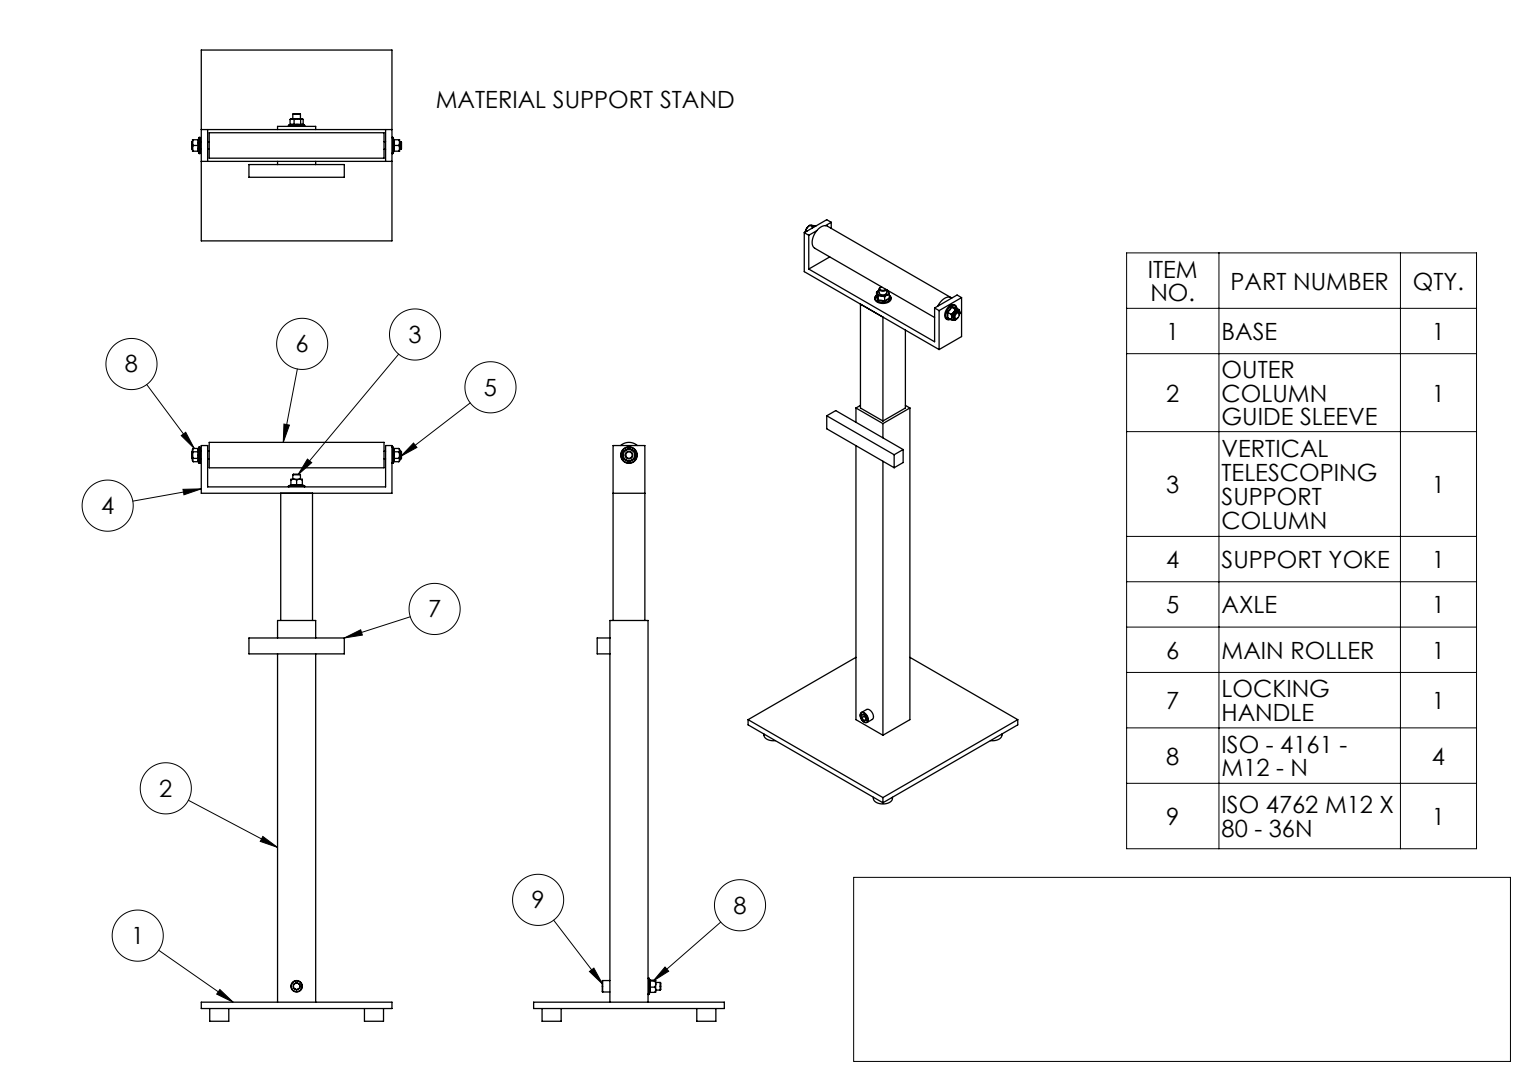
ISO-10303-21;
HEADER;
FILE_DESCRIPTION (('STEP AP214'),
    '1' );
FILE_NAME ('MAS-195',
    '2026-10-22T16:49:52',
    ( '' ),
    ( '' ),
    'SwSTEP 2.0',
    'SolidWorks 2026',
    '' );
FILE_SCHEMA (( 'AUTOMOTIVE_DESIGN' ));
ENDSEC;

DATA;
#1 = CARTESIAN_POINT ( 'NONE',  ( 6.000000000000000000, 5.839897972853065333, -6.938893903907228378E-15 ) ) ;
#2 = EDGE_LOOP ( 'NONE', ( #5035, #4306, #1396, #717 ) ) ;
#3 = ADVANCED_FACE ( 'NONE', ( #4862, #2431 ), #2781, .T. ) ;
#4 =( LENGTH_UNIT ( ) NAMED_UNIT ( * ) SI_UNIT ( .MILLI., .METRE. ) );
#5 = ORIENTED_EDGE ( 'NONE', *, *, #3129, .F. ) ;
#6 = AXIS2_PLACEMENT_3D ( 'NONE', #4882, #5186, #2714 ) ;
#7 = DIRECTION ( 'NONE',  ( 0.000000000000000000, 0.000000000000000000, -1.000000000000000000 ) ) ;
#8 = DIRECTION ( 'NONE',  ( -1.000000000000000000, -0.000000000000000000, -0.000000000000000000 ) ) ;
#9 = DIRECTION ( 'NONE',  ( 1.000000000000000000, -0.000000000000000000, 0.000000000000000000 ) ) ;
#10 = CONTEXT_DEPENDENT_SHAPE_REPRESENTATION ( #2601, #2272 ) ;
#11 = EDGE_CURVE ( 'NONE', #3738, #432, #4098, .T. ) ;
#12 = ORIENTED_EDGE ( 'NONE', *, *, #4828, .T. ) ;
#13 = DIRECTION ( 'NONE',  ( 7.401486830834378251E-16, -1.000000000000000000, 0.000000000000000000 ) ) ;
#14 = FACE_OUTER_BOUND ( 'NONE', #5143, .T. ) ;
#15 = DIRECTION ( 'NONE',  ( -1.000000000000000000, -0.000000000000000000, -0.000000000000000000 ) ) ;
#16 = EDGE_CURVE ( 'NONE', #5260, #261, #3181, .T. ) ;
#17 = CARTESIAN_POINT ( 'NONE',  ( 5.999999999999999112, -6.928203230275514102, -8.505011083697299412 ) ) ;
#18 = PRODUCT_DEFINITION_SHAPE ( 'NONE', 'NONE',  #4920 ) ;
#19 = APPLICATION_CONTEXT ( 'automotive_design' ) ;
#20 = EDGE_LOOP ( 'NONE', ( #1630, #2560 ) ) ;
#21 = CARTESIAN_POINT ( 'NONE',  ( 9.000000000000000000, -5.196152422706636465, -8.935996291721336249 ) ) ;
#22 = DIRECTION ( 'NONE',  ( -0.5000000000000046629, 1.060575238724903587E-16, -0.8660254037844359321 ) ) ;
#23 = ORIENTED_EDGE ( 'NONE', *, *, #198, .T. ) ;
#24 = EDGE_LOOP ( 'NONE', ( #1798, #2180 ) ) ;
#25 = CARTESIAN_POINT ( 'NONE',  ( 121.7157287525372311, 0.000000000000000000, -121.7157287525388369 ) ) ;
#26 = EDGE_LOOP ( 'NONE', ( #4357, #319, #2508, #4041 ) ) ;
#27 = ORIENTED_EDGE ( 'NONE', *, *, #3576, .T. ) ;
#28 = EDGE_LOOP ( 'NONE', ( #1037, #4864, #2855, #4479 ) ) ;
#29 = DIRECTION ( 'NONE',  ( 0.000000000000000000, -1.000000000000000000, 0.000000000000000000 ) ) ;
#30 = CARTESIAN_POINT ( 'NONE',  ( 150.0000000000000000, 810.0000000000000000, 25.00000000000000000 ) ) ;
#31 = CARTESIAN_POINT ( 'NONE',  ( 9.417977369734737536, -4.954833075775112228, -9.021743230619932774 ) ) ;
#32 = DIRECTION ( 'NONE',  ( 1.000000000000000000, -0.000000000000000000, 6.938893903907228378E-17 ) ) ;
#33 = EDGE_LOOP ( 'NONE', ( #4983, #5227 ) ) ;
#34 = DIRECTION ( 'NONE',  ( 1.000000000000000000, 0.000000000000000000, 0.000000000000000000 ) ) ;
#35 = SURFACE_SIDE_STYLE ('',( #3970 ) ) ;
#36 = LINE ( 'NONE', #4185, #4654 ) ;
#37 = CARTESIAN_POINT ( 'NONE',  ( -74.99999999999998579, 610.0000000000000000, 49.99999999999998579 ) ) ;
#38 = TOROIDAL_SURFACE ( 'NONE', #2294, 6.600000000000001421, 0.5999999999999999778 ) ;
#39 = EDGE_CURVE ( 'NONE', #183, #4714, #3882, .T. ) ;
#40 = AXIS2_PLACEMENT_3D ( 'NONE', #2568, #2148, #4717 ) ;
#41 = ORIENTED_EDGE ( 'NONE', *, *, #794, .F. ) ;
#42 = CARTESIAN_POINT ( 'NONE',  ( 149.9999999999999716, 10.00000000000000000, 149.9999999999999716 ) ) ;
#43 = CARTESIAN_POINT ( 'NONE',  ( 8.716942385998452281, -5.934590066575466061, -9.518277236634762772 ) ) ;
#44 = EDGE_LOOP ( 'NONE', ( #3924, #827, #3018, #2315, #3329 ) ) ;
#45 = EDGE_LOOP ( 'NONE', ( #4536, #2353, #4861, #2749 ) ) ;
#46 = VECTOR ( 'NONE', #2795, 1000.000000000000000 ) ;
#47 = MANIFOLD_SOLID_BREP ( 'M12 Machine Threads Stud2', #1956 ) ;
#48 = ORIENTED_EDGE ( 'NONE', *, *, #2007, .T. ) ;
#49 = CIRCLE ( 'NONE', #3968, 20.00000000000001421 ) ;
#50 = CARTESIAN_POINT ( 'NONE',  ( -150.0000000000000000, 870.0000000000000000, 0.000000000000000000 ) ) ;
#51 = VECTOR ( 'NONE', #3265, 1000.000000000000000 ) ;
#52 = EDGE_CURVE ( 'NONE', #4486, #4891, #4610, .T. ) ;
#53 = EDGE_LOOP ( 'NONE', ( #12, #4860, #912, #4381 ) ) ;
#54 = AXIS2_PLACEMENT_3D ( 'NONE', #1971, #1612, #2923 ) ;
#55 = DIRECTION ( 'NONE',  ( 0.000000000000000000, -0.000000000000000000, 1.000000000000000000 ) ) ;
#56 = CARTESIAN_POINT ( 'NONE',  ( -5.303004762135290484, 7.330613618480585458, -8.460795847313656637 ) ) ;
#57 = LINE ( 'NONE', #1683, #3118 ) ;
#58 = ADVANCED_FACE ( 'NONE', ( #1562 ), #1695, .F. ) ;
#59 = CIRCLE ( 'NONE', #3730, 6.499999999999983125 ) ;
#60 = CIRCLE ( 'NONE', #4076, 6.600000000000001421 ) ;
#61 = CARTESIAN_POINT ( 'NONE',  ( -24.99999999999999645, 810.0000000000000000, -25.00000000000000000 ) ) ;
#62 = DIRECTION ( 'NONE',  ( -0.000000000000000000, -0.000000000000000000, 1.000000000000000000 ) ) ;
#63 = CARTESIAN_POINT ( 'NONE',  ( 137.5000000000000000, 870.0000000000000000, 6.000000000000006217 ) ) ;
#64 = DIRECTION ( 'NONE',  ( -0.000000000000000000, -0.000000000000000000, 1.000000000000000000 ) ) ;
#65 = LINE ( 'NONE', #137, #1780 ) ;
#66 = EDGE_LOOP ( 'NONE', ( #727, #5386, #2171, #4175 ) ) ;
#67=STYLED_ITEM('',(#5412),#3780);
#68 = SURFACE_STYLE_FILL_AREA ( #524 ) ;
#69 = EDGE_CURVE ( 'NONE', #3352, #3493, #3834, .T. ) ;
#70 = VECTOR ( 'NONE', #4320, 1000.000000000000000 ) ;
#71 = EDGE_LOOP ( 'NONE', ( #1973, #4142, #2111, #5305 ) ) ;
#72 = CARTESIAN_POINT ( 'NONE',  ( -150.0000000000000000, 820.0000000000001137, 25.00000000000000000 ) ) ;
#73 = DIRECTION ( 'NONE',  ( 0.000000000000000000, 0.000000000000000000, -1.000000000000000000 ) ) ;
#74 = DIRECTION ( 'NONE',  ( 1.000000000000000000, 0.000000000000000000, 0.000000000000000000 ) ) ;
#75 = ORIENTED_EDGE ( 'NONE', *, *, #1128, .F. ) ;
#76 = CIRCLE ( 'NONE', #4758, 20.00000000000001421 ) ;
#77 = AXIS2_PLACEMENT_3D ( 'NONE', #4332, #3953, #3470 ) ;
#78 = DIRECTION ( 'NONE',  ( -6.938893903907228378E-17, 0.000000000000000000, 1.000000000000000000 ) ) ;
#79 = EDGE_CURVE ( 'NONE', #3280, #3385, #2552, .T. ) ;
#80 = EDGE_CURVE ( 'NONE', #4039, #3851, #2630, .T. ) ;
#81 = VERTEX_POINT ( 'NONE', #3427 ) ;
#82 = ORIENTED_EDGE ( 'NONE', *, *, #2566, .T. ) ;
#83 = LINE ( 'NONE', #4223, #2397 ) ;
#84 = DIRECTION ( 'NONE',  ( 2.081668171172168513E-16, 0.000000000000000000, -1.000000000000000000 ) ) ;
#85 = FACE_OUTER_BOUND ( 'NONE', #3426, .T. ) ;
#86 = CARTESIAN_POINT ( 'NONE',  ( -0.3334815747005946962, -10.58484052233643702, -9.543752552345290852 ) ) ;
#87 = CARTESIAN_POINT ( 'NONE',  ( -17.99999999999999645, -3.469446951953614189E-15, 0.000000000000000000 ) ) ;
#88 = LINE ( 'NONE', #3399, #4556 ) ;
#89 = DIRECTION ( 'NONE',  ( 1.000000000000000000, 0.000000000000000000, 0.000000000000000000 ) ) ;
#90 = CARTESIAN_POINT ( 'NONE',  ( 0.000000000000000000, 0.000000000000000000, -12.00000000000000000 ) ) ;
#91 = CARTESIAN_POINT ( 'NONE',  ( 5.099999999999999645, 0.000000000000000000, -0.6301867843887398735 ) ) ;
#92 = ORIENTED_EDGE ( 'NONE', *, *, #352, .F. ) ;
#93 = DIRECTION ( 'NONE',  ( -1.000000000000000000, -0.000000000000000000, -0.000000000000000000 ) ) ;
#94 = CARTESIAN_POINT ( 'NONE',  ( 7.780966735391740663, 5.899961606179080498, -9.200452032548549042 ) ) ;
#95 = UNCERTAINTY_MEASURE_WITH_UNIT (LENGTH_MEASURE( 1.000000000000000082E-05 ), #3819, 'distance_accuracy_value', 'NONE');
#96 = CARTESIAN_POINT ( 'NONE',  ( 3.148120153201419136, -9.125992800952634099, -9.189707035345831443 ) ) ;
#97 = CARTESIAN_POINT ( 'NONE',  ( 0.000000000000000000, 810.0000000000000000, 0.000000000000000000 ) ) ;
#98 = EDGE_CURVE ( 'NONE', #1888, #3300, #2243, .T. ) ;
#99 = ORIENTED_EDGE ( 'NONE', *, *, #4103, .T. ) ;
#100 = CARTESIAN_POINT ( 'NONE',  ( 0.000000000000000000, 0.000000000000000000, 0.000000000000000000 ) ) ;
#101 = DIRECTION ( 'NONE',  ( 0.000000000000000000, 0.000000000000000000, 1.000000000000000000 ) ) ;
#102 = CARTESIAN_POINT ( 'NONE',  ( 24.99999999999999645, 60.00000000000000711, -25.00000000000000000 ) ) ;
#103 = DIRECTION ( 'NONE',  ( 1.000000000000000000, 0.000000000000000000, 0.000000000000000000 ) ) ;
#104 = MANIFOLD_SOLID_BREP ( 'M12 Clearance Hole1', #2049 ) ;
#105 = CARTESIAN_POINT ( 'NONE',  ( 9.506737344437272696, -5.488717364925930653, -9.686084310752812954 ) ) ;
#106 = DIRECTION ( 'NONE',  ( 1.000000000000000000, 0.000000000000000000, 0.000000000000000000 ) ) ;
#107 = CARTESIAN_POINT ( 'NONE',  ( -3.715831927071960639, 8.246968282054856658, 1.905824131322174974E-15 ) ) ;
#108 = LINE ( 'NONE', #1461, #5040 ) ;
#109 = APPLICATION_CONTEXT ( 'automotive_design' ) ;
#110 = EDGE_CURVE ( 'NONE', #2103, #3079, #2190, .T. ) ;
#111 = CARTESIAN_POINT ( 'NONE',  ( -150.0000000000000284, 10.00000000000000000, 149.9999999999999147 ) ) ;
#112 = PLANE ( 'NONE',  #5289 ) ;
#113 = CARTESIAN_POINT ( 'NONE',  ( 9.333481574700595473, 5.003616745783458164, -9.543752552345289075 ) ) ;
#114 = DIRECTION ( 'NONE',  ( 1.000000000000000000, 0.000000000000000000, 0.000000000000000000 ) ) ;
#115 = EDGE_CURVE ( 'NONE', #4871, #4344, #3809, .T. ) ;
#116 = VECTOR ( 'NONE', #4178, 1000.000000000000000 ) ;
#117 = CARTESIAN_POINT ( 'NONE',  ( -121.7157287525381122, -20.00000000000000000, 106.7157287525380127 ) ) ;
#118 = CIRCLE ( 'NONE', #3006, 6.499999999999988454 ) ;
#119 = ADVANCED_BREP_SHAPE_REPRESENTATION ( '', ( #1812, #4154 ), #5370 ) ;
#120 = EDGE_LOOP ( 'NONE', ( #3988, #3057, #2483, #2092 ) ) ;
#121 = SHAPE_REPRESENTATION ( 'Locking handle', ( #4154 ), #2227 ) ;
#122 = AXIS2_PLACEMENT_3D ( 'NONE', #2468, #3586, #4820 ) ;
#123 = ORIENTED_EDGE ( 'NONE', *, *, #1408, .F. ) ;
#124 = DIRECTION ( 'NONE',  ( 1.224646799147353207E-16, 1.000000000000000000, 0.000000000000000000 ) ) ;
#125 = CARTESIAN_POINT ( 'NONE',  ( 92.00000000000000000, 0.000000000000000000, 5.035999999999999588 ) ) ;
#126 = EDGE_CURVE ( 'NONE', #4344, #870, #2364, .T. ) ;
#127 = DIRECTION ( 'NONE',  ( -0.000000000000000000, -0.000000000000000000, 1.000000000000000000 ) ) ;
#128 = VECTOR ( 'NONE', #1979, 1000.000000000000000 ) ;
#129 = CIRCLE ( 'NONE', #3889, 6.000000000000000000 ) ;
#130 = AXIS2_PLACEMENT_3D ( 'NONE', #2726, #4867, #1140 ) ;
#131 = CARTESIAN_POINT ( 'NONE',  ( -8.999999999999998224, 4.786605659887710473, -1.023509873932516578 ) ) ;
#132 = CARTESIAN_POINT ( 'NONE',  ( 165.0000000000000000, 870.0000000000000000, -5.036000000000040444 ) ) ;
#133 = DIRECTION ( 'NONE',  ( 1.000000000000000000, 0.000000000000000000, 0.000000000000000000 ) ) ;
#134 = CARTESIAN_POINT ( 'NONE',  ( 30.00000000000000355, 610.0000000000000000, 30.00000000000001066 ) ) ;
#135 = ORIENTED_EDGE ( 'NONE', *, *, #3214, .F. ) ;
#136 = EDGE_CURVE ( 'NONE', #4283, #3488, #3860, .T. ) ;
#137 = CARTESIAN_POINT ( 'NONE',  ( -24.99999999999999645, 610.0000000000000000, -25.00000000000000000 ) ) ;
#138 = DIRECTION ( 'NONE',  ( 0.000000000000000000, 0.000000000000000000, 1.000000000000000000 ) ) ;
#139 = EDGE_CURVE ( 'NONE', #2539, #1113, #5108, .T. ) ;
#140 = AXIS2_PLACEMENT_3D ( 'NONE', #4031, #279, #2385 ) ;
#141 = COLOUR_RGB ( '',0.8941176470588234615, 0.8941176470588234615, 0.8941176470588234615 ) ;
#142 = CARTESIAN_POINT ( 'NONE',  ( 6.000000000000000000, 5.839897972853065333, -6.938893903907228378E-15 ) ) ;
#143 = DIRECTION ( 'NONE',  ( 0.000000000000000000, 0.000000000000000000, -1.000000000000000000 ) ) ;
#144 = CARTESIAN_POINT ( 'NONE',  ( 0.000000000000000000, 570.0000000000000000, 25.00000000000000000 ) ) ;
#145 = VECTOR ( 'NONE', #5158, 1000.000000000000000 ) ;
#146 = CARTESIAN_POINT ( 'NONE',  ( -74.99999999999998579, 582.4999999999997726, 49.99999999999998579 ) ) ;
#147 = CARTESIAN_POINT ( 'NONE',  ( -121.7157287525381122, 0.000000000000000000, 106.7157287525380127 ) ) ;
#148 = VECTOR ( 'NONE', #4543, 1000.000000000000000 ) ;
#149 = CARTESIAN_POINT ( 'NONE',  ( 0.000000000000000000, -2.919948986426539772, -5.057499999999996554 ) ) ;
#150 = VECTOR ( 'NONE', #4769, 1000.000000000000000 ) ;
#151 = ORIENTED_EDGE ( 'NONE', *, *, #3972, .F. ) ;
#152 = SURFACE_STYLE_USAGE ( .BOTH. , #2636 ) ;
#153 = ORIENTED_EDGE ( 'NONE', *, *, #5054, .F. ) ;
#154 = VECTOR ( 'NONE', #5264, 1000.000000000000000 ) ;
#155 = ORIENTED_EDGE ( 'NONE', *, *, #2076, .F. ) ;
#156 = EDGE_CURVE ( 'NONE', #870, #4344, #3054, .T. ) ;
#157 = SURFACE_SIDE_STYLE ('',( #4715 ) ) ;
#158 = LINE ( 'NONE', #4749, #4217 ) ;
#159 = CARTESIAN_POINT ( 'NONE',  ( 6.000000000000000000, -5.258101095580057102E-15, -5.057500000000000107 ) ) ;
#160 = ORIENTED_EDGE ( 'NONE', *, *, #3298, .F. ) ;
#161 = ORIENTED_EDGE ( 'NONE', *, *, #5198, .T. ) ;
#162 = CARTESIAN_POINT ( 'NONE',  ( -150.0000000000000000, 870.0000000000000000, -6.000000000000006217 ) ) ;
#163 = FACE_OUTER_BOUND ( 'NONE', #2172, .T. ) ;
#164 = DIRECTION ( 'NONE',  ( -0.000000000000000000, -0.000000000000000000, 1.000000000000000000 ) ) ;
#165 = VERTEX_POINT ( 'NONE', #2690 ) ;
#166 = CARTESIAN_POINT ( 'NONE',  ( 9.000000000000000000, -5.196152422706636465, -8.935996291721336249 ) ) ;
#167 = EDGE_CURVE ( 'NONE', #2868, #5294, #475, .T. ) ;
#168 = CARTESIAN_POINT ( 'NONE',  ( 8.999999999999998224, -3.085342593989931714, -0.4353033105082919074 ) ) ;
#169 = ORIENTED_EDGE ( 'NONE', *, *, #1169, .T. ) ;
#170 = DIRECTION ( 'NONE',  ( 0.000000000000000000, -0.5000000000000012212, -0.8660254037844380415 ) ) ;
#171 = CARTESIAN_POINT ( 'NONE',  ( 5.010000000000002451, 0.000000000000000000, -0.6932054628276118624 ) ) ;
#172 = MECHANICAL_DESIGN_GEOMETRIC_PRESENTATION_REPRESENTATION (  '', ( #4869 ), #4866 ) ;
#173 = CARTESIAN_POINT ( 'NONE',  ( 12.38940648156203927, 1.517264699098042146E-15, -10.20000000000000107 ) ) ;
#174 = DIRECTION ( 'NONE',  ( -1.000000000000000000, 0.000000000000000000, 0.000000000000000000 ) ) ;
#175 = CARTESIAN_POINT ( 'NONE',  ( 8.999999999999998224, 5.582890641074283344, -9.544071791823135698 ) ) ;
#176 = CARTESIAN_POINT ( 'NONE',  ( 7.500000000000000000, 6.062177826491069510, -8.667800885990208926 ) ) ;
#177 = ORIENTED_EDGE ( 'NONE', *, *, #2712, .T. ) ;
#178 =( NAMED_UNIT ( * ) SI_UNIT ( $, .STERADIAN. ) SOLID_ANGLE_UNIT ( ) );
#179 = EDGE_CURVE ( 'NONE', #353, #1195, #2907, .T. ) ;
#180 = CARTESIAN_POINT ( 'NONE',  ( 0.000000000000000000, 0.000000000000000000, 0.000000000000000000 ) ) ;
#181 = CARTESIAN_POINT ( 'NONE',  ( 0.000000000000000000, 450.0000000000000000, 25.00000000000000000 ) ) ;
#182 = PRODUCT_DEFINITION ( 'UNKNOWN', '', #3186, #2002 ) ;
#183 = VERTEX_POINT ( 'NONE', #3483 ) ;
#184 = CARTESIAN_POINT ( 'NONE',  ( -121.7157287525381122, 0.000000000000000000, 121.7157287525380127 ) ) ;
#185 = CARTESIAN_POINT ( 'NONE',  ( -9.000000000000000000, 5.196152422706629359, -8.935996291721334472 ) ) ;
#186 = LINE ( 'NONE', #5103, #588 ) ;
#187 = CARTESIAN_POINT ( 'NONE',  ( 162.0000000000000000, 870.0000000000000000, 0.000000000000000000 ) ) ;
#188 = EDGE_LOOP ( 'NONE', ( #4329, #3309, #4220, #3176 ) ) ;
#189 = DIRECTION ( 'NONE',  ( -1.000000000000000000, -0.000000000000000000, -0.000000000000000000 ) ) ;
#190 = SURFACE_STYLE_FILL_AREA ( #1881 ) ;
#191 = DIRECTION ( 'NONE',  ( -0.000000000000000000, -1.000000000000000000, 0.000000000000000000 ) ) ;
#192 = DIRECTION ( 'NONE',  ( -0.000000000000000000, 1.000000000000000000, -0.000000000000000000 ) ) ;
#193 = FACE_OUTER_BOUND ( 'NONE', #4538, .T. ) ;
#194 = EDGE_CURVE ( 'NONE', #2394, #3572, #803, .T. ) ;
#195 = CARTESIAN_POINT ( 'NONE',  ( 165.0000000000000000, 870.0000000000000000, 5.036000000000040444 ) ) ;
#196 = DIRECTION ( 'NONE',  ( -0.000000000000000000, 1.000000000000000000, -0.000000000000000000 ) ) ;
#197 = ORIENTED_EDGE ( 'NONE', *, *, #3520, .F. ) ;
#198 = EDGE_CURVE ( 'NONE', #3942, #4623, #5254, .T. ) ;
#199 = CONICAL_SURFACE ( 'NONE', #1255, 5.036000000000040444, 0.7853981633974339571 ) ;
#200 = ORIENTED_EDGE ( 'NONE', *, *, #4627, .T. ) ;
#201 = CARTESIAN_POINT ( 'NONE',  ( 121.7157287525384533, -20.00000000000000000, 121.7157287525376859 ) ) ;
#202 = ORIENTED_EDGE ( 'NONE', *, *, #4322, .T. ) ;
#203 = DIRECTION ( 'NONE',  ( 0.000000000000000000, 0.000000000000000000, -1.000000000000000000 ) ) ;
#204 = CARTESIAN_POINT ( 'NONE',  ( 0.000000000000000000, 450.0000000000000000, -25.00000000000000000 ) ) ;
#205 = COLOUR_RGB ( '',1.000000000000000000, 0.9490196078431372140, 0.9098039215686274384 ) ;
#206 = EDGE_CURVE ( 'NONE', #3842, #5043, #2268, .T. ) ;
#207 = VERTEX_POINT ( 'NONE', #1151 ) ;
#208 = AXIS2_PLACEMENT_3D ( 'NONE', #1676, #429, #2877 ) ;
#209 = CARTESIAN_POINT ( 'NONE',  ( -9.506737344437272696, 5.488717364925923548, -9.686084310752812954 ) ) ;
#210 = CARTESIAN_POINT ( 'NONE',  ( 5.035999999999999588, 840.0000000000001137, 0.000000000000000000 ) ) ;
#211 = EDGE_CURVE ( 'NONE', #2103, #3135, #3145, .T. ) ;
#212 = ADVANCED_FACE ( 'NONE', ( #4821, #5247 ), #1493, .F. ) ;
#213 = DIRECTION ( 'NONE',  ( -1.000000000000000000, 0.000000000000000000, -2.081668171172168513E-16 ) ) ;
#214 = CARTESIAN_POINT ( 'NONE',  ( 9.000000000000007105, -5.196152422706631135, -9.106324069981642566 ) ) ;
#215 = FILL_AREA_STYLE ('',( #650 ) ) ;
#216 = AXIS2_PLACEMENT_3D ( 'NONE', #2652, #2351, #4049 ) ;
#217 = CIRCLE ( 'NONE', #2845, 6.499999999999988454 ) ;
#218 = PRESENTATION_LAYER_ASSIGNMENT (  '', '', ( #3627 ) ) ;
#219 = CARTESIAN_POINT ( 'NONE',  ( 8.919948986426568638, 0.000000000000000000, 0.000000000000000000 ) ) ;
#220 = ORIENTED_EDGE ( 'NONE', *, *, #4751, .F. ) ;
#221 = CARTESIAN_POINT ( 'NONE',  ( -3.936978610624180419, -8.666338374798538524, -9.138972935415381471 ) ) ;
#222 = CARTESIAN_POINT ( 'NONE',  ( 4.105894441359817293, 8.021765584429983775, 1.987139294258588595E-15 ) ) ;
#223 = ADVANCED_FACE ( 'NONE', ( #720 ), #3527, .F. ) ;
#224 = DIRECTION ( 'NONE',  ( 0.000000000000000000, 0.000000000000000000, -1.000000000000000000 ) ) ;
#225 = DIRECTION ( 'NONE',  ( -0.000000000000000000, 1.000000000000000000, -0.000000000000000000 ) ) ;
#226 = CIRCLE ( 'NONE', #1785, 6.499999999999988454 ) ;
#227 =( GEOMETRIC_REPRESENTATION_CONTEXT ( 3 ) GLOBAL_UNCERTAINTY_ASSIGNED_CONTEXT ( ( #1775 ) ) GLOBAL_UNIT_ASSIGNED_CONTEXT ( ( #3570, #5196, #2363 ) ) REPRESENTATION_CONTEXT ( 'NONE', 'WORKASPACE' ) );
#228 = AXIS2_PLACEMENT_3D ( 'NONE', #622, #648, #2683 ) ;
#229 = MECHANICAL_DESIGN_GEOMETRIC_PRESENTATION_REPRESENTATION (  '', ( #3546 ), #1970 ) ;
#230 = CARTESIAN_POINT ( 'NONE',  ( 9.000000000000000000, -1.974011471328773748, -8.465140122390733879 ) ) ;
#231 = PLANE ( 'NONE',  #3894 ) ;
#232 = VECTOR ( 'NONE', #2038, 1000.000000000000000 ) ;
#233 = EDGE_CURVE ( 'NONE', #932, #4959, #723, .T. ) ;
#234 = VECTOR ( 'NONE', #2330, 1000.000000000000000 ) ;
#235 = ORIENTED_EDGE ( 'NONE', *, *, #3529, .T. ) ;
#236 = CYLINDRICAL_SURFACE ( 'NONE', #2573, 6.499999999999983125 ) ;
#237 = ADVANCED_FACE ( 'NONE', ( #3202, #2295 ), #602, .T. ) ;
#238 = ORIENTED_EDGE ( 'NONE', *, *, #1651, .F. ) ;
#239 = DIRECTION ( 'NONE',  ( -1.000000000000000000, -0.000000000000000000, -0.000000000000000000 ) ) ;
#240 = FACE_OUTER_BOUND ( 'NONE', #4695, .T. ) ;
#241 = AXIS2_PLACEMENT_3D ( 'NONE', #2577, #882, #3403 ) ;
#242 = ORIENTED_EDGE ( 'NONE', *, *, #1915, .F. ) ;
#243 = DIRECTION ( 'NONE',  ( -1.000000000000000000, -0.000000000000000000, -0.000000000000000000 ) ) ;
#244 = CARTESIAN_POINT ( 'NONE',  ( -6.177322775498885754, -6.825825878106156708, -8.969375302469426714 ) ) ;
#245 = CIRCLE ( 'NONE', #77, 6.000000000000006217 ) ;
#246 = CARTESIAN_POINT ( 'NONE',  ( 6.000000000000000000, -5.839897972853064445, 4.770489558936219510E-15 ) ) ;
#247 = CARTESIAN_POINT ( 'NONE',  ( 139.9999999999999716, 885.0000000000000000, -25.00000000000000000 ) ) ;
#248 = DIRECTION ( 'NONE',  ( 0.000000000000000000, 0.000000000000000000, 1.000000000000000000 ) ) ;
#249 = ORIENTED_EDGE ( 'NONE', *, *, #342, .F. ) ;
#250 = CARTESIAN_POINT ( 'NONE',  ( 9.000000000000000000, -4.368650009232623255, -0.8589767385557531831 ) ) ;
#251 = CARTESIAN_POINT ( 'NONE',  ( 0.000000000000000000, 0.000000000000000000, 0.000000000000000000 ) ) ;
#252 = CARTESIAN_POINT ( 'NONE',  ( -0.7813822207450746848, 10.51618336147351584, -9.518202542148552325 ) ) ;
#253 = DIRECTION ( 'NONE',  ( 1.000000000000000000, 0.000000000000000000, 0.000000000000000000 ) ) ;
#254 = CARTESIAN_POINT ( 'NONE',  ( -150.0000000000000284, 0.000000000000000000, 149.9999999999999147 ) ) ;
#255 = PRODUCT_DEFINITION ( 'UNKNOWN', '', #483, #2329 ) ;
#256 = CARTESIAN_POINT ( 'NONE',  ( 8.999999999999998224, 3.726892940488169881, -9.220324059310399889 ) ) ;
#257 = CARTESIAN_POINT ( 'NONE',  ( 30.00000000000000355, 610.0000000000000000, 30.00000000000001066 ) ) ;
#258 = MANIFOLD_SOLID_BREP ( 'M12 Machine Threads Stud1', #3451 ) ;
#259 = ORIENTED_EDGE ( 'NONE', *, *, #2872, .T. ) ;
#260 = FACE_OUTER_BOUND ( 'NONE', #4753, .T. ) ;
#261 = VERTEX_POINT ( 'NONE', #1126 ) ;
#262 = DIRECTION ( 'NONE',  ( 1.000000000000000000, 0.000000000000000000, 0.000000000000000000 ) ) ;
#263 = DIRECTION ( 'NONE',  ( 0.000000000000000000, 0.000000000000000000, 1.000000000000000000 ) ) ;
#264 = ADVANCED_FACE ( 'NONE', ( #307 ), #2257, .T. ) ;
#265 = EDGE_LOOP ( 'NONE', ( #2371, #2953, #3859, #3002, #619 ) ) ;
#266 = EDGE_CURVE ( 'NONE', #4086, #2529, #4435, .T. ) ;
#267 = ORIENTED_EDGE ( 'NONE', *, *, #3062, .T. ) ;
#268 = CARTESIAN_POINT ( 'NONE',  ( -12.07201791628681420, 1.497830254570528423E-15, -12.00000000000000178 ) ) ;
#269 = DIRECTION ( 'NONE',  ( 0.000000000000000000, 0.000000000000000000, -1.000000000000000000 ) ) ;
#270 = CARTESIAN_POINT ( 'NONE',  ( 9.473745496805531019, 0.9193675319299579041, -9.138786188337409300 ) ) ;
#271 = CARTESIAN_POINT ( 'NONE',  ( 6.499999999999988454, 450.0000000000000000, -25.00000000000000000 ) ) ;
#272 = APPLICATION_PROTOCOL_DEFINITION ( 'draft international standard', 'automotive_design', 1998, #5061 ) ;
#273 = VERTEX_POINT ( 'NONE', #4446 ) ;
#274 = B_SPLINE_CURVE_WITH_KNOTS ( 'NONE', 3,
 ( #1691, #107, #2527, #1724, #4580, #2576 ),
 .UNSPECIFIED., .F., .F.,
 ( 4, 2, 4 ),
 ( 0.005333245961717295557, 0.007986067645924077585, 0.01063888933013085875 ),
 .UNSPECIFIED. ) ;
#275 = DIRECTION ( 'NONE',  ( 1.000000000000000000, 0.000000000000000000, 0.000000000000000000 ) ) ;
#276 = ORIENTED_EDGE ( 'NONE', *, *, #1791, .T. ) ;
#277 = CARTESIAN_POINT ( 'NONE',  ( -3.145304002162441659, -9.127642243957643231, -9.190020220263408035 ) ) ;
#278 = CYLINDRICAL_SURFACE ( 'NONE', #4326, 9.000000000000000000 ) ;
#279 = DIRECTION ( 'NONE',  ( -0.000000000000000000, -0.000000000000000000, 1.000000000000000000 ) ) ;
#280 = CARTESIAN_POINT ( 'NONE',  ( 139.9999999999999716, 885.0000000000000000, 25.00000000000000000 ) ) ;
#281 = ADVANCED_FACE ( 'NONE', ( #2796 ), #733, .T. ) ;
#282 = LINE ( 'NONE', #1853, #2054 ) ;
#283 = DIRECTION ( 'NONE',  ( -0.000000000000000000, -0.000000000000000000, 1.000000000000000000 ) ) ;
#284 = EDGE_CURVE ( 'NONE', #3602, #4122, #385, .T. ) ;
#285 = VERTEX_POINT ( 'NONE', #3734 ) ;
#286 = EDGE_LOOP ( 'NONE', ( #1725, #726, #2392, #4939 ) ) ;
#287 = APPLICATION_CONTEXT ( 'automotive_design' ) ;
#288 = PRESENTATION_STYLE_ASSIGNMENT (( #4836 ) ) ;
#289 = DIRECTION ( 'NONE',  ( 0.000000000000000000, 0.000000000000000000, 1.000000000000000000 ) ) ;
#290 = AXIS2_PLACEMENT_3D ( 'NONE', #2542, #2961, #4599 ) ;
#291 = EDGE_LOOP ( 'NONE', ( #3664, #547 ) ) ;
#292 = DIRECTION ( 'NONE',  ( -0.5000000000000004441, 0.8660254037844384856, 0.000000000000000000 ) ) ;
#293 = FACE_OUTER_BOUND ( 'NONE', #4919, .T. ) ;
#294 = EDGE_LOOP ( 'NONE', ( #2275, #2236, #92, #4689 ) ) ;
#295 = AXIS2_PLACEMENT_3D ( 'NONE', #2964, #518, #4278 ) ;
#296 = ORIENTED_EDGE ( 'NONE', *, *, #4163, .F. ) ;
#297 = DIRECTION ( 'NONE',  ( 0.000000000000000000, -1.000000000000000000, 0.000000000000000000 ) ) ;
#298 = CARTESIAN_POINT ( 'NONE',  ( 164.0360000000000014, 870.0000000000000000, -6.000000000000006217 ) ) ;
#299 = DIRECTION ( 'NONE',  ( -0.000000000000000000, -0.000000000000000000, 1.000000000000000000 ) ) ;
#300 = VECTOR ( 'NONE', #2784, 1000.000000000000000 ) ;
#301 = UNCERTAINTY_MEASURE_WITH_UNIT (LENGTH_MEASURE( 1.000000000000000082E-05 ), #2011, 'distance_accuracy_value', 'NONE');
#302 = SHAPE_REPRESENTATION ( 'axle', ( #4154 ), #2055 ) ;
#303 = ORIENTED_EDGE ( 'NONE', *, *, #2481, .F. ) ;
#304 = AXIS2_PLACEMENT_3D ( 'NONE', #2018, #4467, #1392 ) ;
#305 = ADVANCED_FACE ( 'NONE', ( #1215, #3776 ), #1663, .T. ) ;
#306 = DIRECTION ( 'NONE',  ( 1.000000000000000000, 0.000000000000000000, -0.000000000000000000 ) ) ;
#307 = FACE_OUTER_BOUND ( 'NONE', #4376, .T. ) ;
#308 = SURFACE_STYLE_USAGE ( .BOTH. , #4112 ) ;
#309 = CARTESIAN_POINT ( 'NONE',  ( -137.5000000000000000, 870.0000000000000000, 0.000000000000000000 ) ) ;
#310 = EDGE_CURVE ( 'NONE', #3078, #932, #2677, .T. ) ;
#311 = DIRECTION ( 'NONE',  ( -0.000000000000000000, -0.000000000000000000, 1.000000000000000000 ) ) ;
#312 = CIRCLE ( 'NONE', #208, 6.000000000000005329 ) ;
#313 = PRODUCT ( 'base', 'base', '', ( #3317 ) ) ;
#314 = VECTOR ( 'NONE', #1467, 1000.000000000000000 ) ;
#315 =( GEOMETRIC_REPRESENTATION_CONTEXT ( 3 ) GLOBAL_UNCERTAINTY_ASSIGNED_CONTEXT ( ( #477 ) ) GLOBAL_UNIT_ASSIGNED_CONTEXT ( ( #4680, #2127, #929 ) ) REPRESENTATION_CONTEXT ( 'NONE', 'WORKASPACE' ) );
#316 = CARTESIAN_POINT ( 'NONE',  ( 121.7157287525384533, -20.00000000000000000, 121.7157287525376859 ) ) ;
#317 = PLANE ( 'NONE',  #5199 ) ;
#318 = SHAPE_REPRESENTATION_RELATIONSHIP ( 'NONE' , 'NONE' ,  #302, #3330 ) ;
#319 = ORIENTED_EDGE ( 'NONE', *, *, #4633, .F. ) ;
#320 = ORIENTED_EDGE ( 'NONE', *, *, #1915, .T. ) ;
#321 = AXIS2_PLACEMENT_3D ( 'NONE', #748, #4422, #1239 ) ;
#322 = ORIENTED_EDGE ( 'NONE', *, *, #3874, .F. ) ;
#323 = DIRECTION ( 'NONE',  ( 0.000000000000000000, 0.000000000000000000, 1.000000000000000000 ) ) ;
#324 = EDGE_LOOP ( 'NONE', ( #2487, #2510, #2629, #3709 ) ) ;
#325 = VECTOR ( 'NONE', #1251, 1000.000000000000000 ) ;
#326 = CIRCLE ( 'NONE', #2598, 6.000000000000000888 ) ;
#327 = VECTOR ( 'NONE', #3004, 1000.000000000000000 ) ;
#328 = EDGE_CURVE ( 'NONE', #745, #5291, #1071, .T. ) ;
#329 = ORIENTED_EDGE ( 'NONE', *, *, #2069, .F. ) ;
#330 = DIRECTION ( 'NONE',  ( 0.000000000000000000, 0.000000000000000000, 1.000000000000000000 ) ) ;
#331 = DIRECTION ( 'NONE',  ( 0.000000000000000000, 0.000000000000000000, -1.000000000000000000 ) ) ;
#332 = DIRECTION ( 'NONE',  ( 0.000000000000000000, 0.000000000000000000, -1.000000000000000000 ) ) ;
#333 = DIRECTION ( 'NONE',  ( -0.000000000000000000, -0.000000000000000000, 1.000000000000000000 ) ) ;
#334 = AXIS2_PLACEMENT_3D ( 'NONE', #394, #283, #1936 ) ;
#335 = SHAPE_DEFINITION_REPRESENTATION ( #2409, #1634 ) ;
#336 = CIRCLE ( 'NONE', #2605, 5.999999999999894307 ) ;
#337 = FACE_OUTER_BOUND ( 'NONE', #718, .T. ) ;
#338 = VERTEX_POINT ( 'NONE', #418 ) ;
#339 = CARTESIAN_POINT ( 'NONE',  ( 165.0000000000000000, 870.0000000000000000, 0.000000000000000000 ) ) ;
#340 = CARTESIAN_POINT ( 'NONE',  ( -3.148120153201420912, 9.125992800952626993, -9.189707035345829667 ) ) ;
#341 = DIRECTION ( 'NONE',  ( -0.000000000000000000, 1.188187522481193495E-15, 1.000000000000000000 ) ) ;
#342 = EDGE_CURVE ( 'NONE', #2324, #5253, #4160, .T. ) ;
#343 = ORIENTED_EDGE ( 'NONE', *, *, #2742, .T. ) ;
#344 = FACE_OUTER_BOUND ( 'NONE', #1476, .T. ) ;
#345 = CARTESIAN_POINT ( 'NONE',  ( 30.00000000000000355, 610.0000000000000000, 0.000000000000000000 ) ) ;
#346 = EDGE_LOOP ( 'NONE', ( #4288, #3328, #1002, #1263, #1161 ) ) ;
#347 = ORIENTED_EDGE ( 'NONE', *, *, #1984, .F. ) ;
#348 = EDGE_LOOP ( 'NONE', ( #4253, #4137 ) ) ;
#349 = CARTESIAN_POINT ( 'NONE',  ( -1.144917494144692998E-14, 570.0000000000000000, -24.99999999999998579 ) ) ;
#350 = DIRECTION ( 'NONE',  ( -1.000000000000000000, -0.000000000000000000, -0.000000000000000000 ) ) ;
#351 = ORIENTED_EDGE ( 'NONE', *, *, #3520, .T. ) ;
#352 = EDGE_CURVE ( 'NONE', #3556, #1113, #326, .T. ) ;
#353 = VERTEX_POINT ( 'NONE', #1576 ) ;
#354 = DIRECTION ( 'NONE',  ( 0.000000000000000000, 0.000000000000000000, -1.000000000000000000 ) ) ;
#355 = CARTESIAN_POINT ( 'NONE',  ( 0.000000000000000000, 810.0000000000000000, 0.000000000000000000 ) ) ;
#356 = DIRECTION ( 'NONE',  ( 0.000000000000000000, -0.000000000000000000, 1.000000000000000000 ) ) ;
#357 = DIRECTION ( 'NONE',  ( 1.000000000000000000, 0.000000000000000000, 0.000000000000000000 ) ) ;
#358 = CONTEXT_DEPENDENT_SHAPE_REPRESENTATION ( #672, #716 ) ;
#359 = DIRECTION ( 'NONE',  ( 0.000000000000000000, 0.000000000000000000, -1.000000000000000000 ) ) ;
#360 = ORIENTED_EDGE ( 'NONE', *, *, #1632, .T. ) ;
#361 = CARTESIAN_POINT ( 'NONE',  ( -2.352990130084610634E-16, 10.39230484541326582, -8.935996291721336249 ) ) ;
#362 = SURFACE_STYLE_FILL_AREA ( #1152 ) ;
#363 = FACE_BOUND ( 'NONE', #348, .T. ) ;
#364 = DIRECTION ( 'NONE',  ( 0.000000000000000000, 0.000000000000000000, -1.000000000000000000 ) ) ;
#365 = EDGE_CURVE ( 'NONE', #3274, #4246, #3257, .T. ) ;
#366 = VERTEX_POINT ( 'NONE', #1238 ) ;
#367 = PLANE ( 'NONE',  #841 ) ;
#368 = CARTESIAN_POINT ( 'NONE',  ( -4.500000000000001776, 7.794228634059948035, -8.419403919045800322 ) ) ;
#369 = ORIENTED_EDGE ( 'NONE', *, *, #1898, .T. ) ;
#370 = ORIENTED_EDGE ( 'NONE', *, *, #1420, .T. ) ;
#371 = DIRECTION ( 'NONE',  ( -0.000000000000000000, -0.000000000000000000, -1.000000000000000000 ) ) ;
#372 = ADVANCED_FACE ( 'NONE', ( #4132 ), #2916, .F. ) ;
#373 = ORIENTED_EDGE ( 'NONE', *, *, #3431, .F. ) ;
#374 = ORIENTED_EDGE ( 'NONE', *, *, #3449, .T. ) ;
#375 = DIRECTION ( 'NONE',  ( 0.000000000000000000, 1.000000000000000000, -1.224646799147353207E-16 ) ) ;
#376 = CARTESIAN_POINT ( 'NONE',  ( 139.9999999999999716, 820.0000000000001137, -25.00000000000000000 ) ) ;
#377 = DIRECTION ( 'NONE',  ( 0.000000000000000000, -0.000000000000000000, -1.000000000000000000 ) ) ;
#378 = CARTESIAN_POINT ( 'NONE',  ( 8.603171985749828110, -5.425261183555956102, -8.848996304169093108 ) ) ;
#379 = APPLICATION_PROTOCOL_DEFINITION ( 'draft international standard', 'automotive_design', 1998, #287 ) ;
#380 = EDGE_CURVE ( 'NONE', #4951, #2954, #3997, .T. ) ;
#381 = AXIS2_PLACEMENT_3D ( 'NONE', #2439, #1631, #3694 ) ;
#382 = CARTESIAN_POINT ( 'NONE',  ( -9.497981232281496489, 4.582241663078505667, -9.518359232022067573 ) ) ;
#383 = CONICAL_SURFACE ( 'NONE', #1593, 5.010000000000002451, 0.9599310885968808105 ) ;
#384 = ORIENTED_EDGE ( 'NONE', *, *, #564, .F. ) ;
#385 = LINE ( 'NONE', #2047, #5346 ) ;
#386 = CARTESIAN_POINT ( 'NONE',  ( -30.00000000000000355, 610.0000000000000000, -2.081668171172168908E-15 ) ) ;
#387 = ADVANCED_BREP_SHAPE_REPRESENTATION ( '', ( #3628, #4154 ), #755 ) ;
#388 = PLANE ( 'NONE',  #3538 ) ;
#389 = CARTESIAN_POINT ( 'NONE',  ( 6.000000000000000000, 5.839897972853065333, -6.938893903907228378E-15 ) ) ;
#390 = VECTOR ( 'NONE', #4500, 1000.000000000000000 ) ;
#391 = EDGE_CURVE ( 'NONE', #2814, #4086, #2436, .T. ) ;
#392 = ORIENTED_EDGE ( 'NONE', *, *, #593, .F. ) ;
#393 = CARTESIAN_POINT ( 'NONE',  ( -6.499999999999988454, 330.0000000000000000, 25.00000000000000000 ) ) ;
#394 = CARTESIAN_POINT ( 'NONE',  ( -1.144917494144692998E-14, 570.0000000000000000, -24.03599999999999071 ) ) ;
#395 = CIRCLE ( 'NONE', #5175, 14.99999999999998579 ) ;
#396 = ORIENTED_EDGE ( 'NONE', *, *, #1896, .F. ) ;
#397 = ORIENTED_EDGE ( 'NONE', *, *, #4687, .F. ) ;
#398 = EDGE_LOOP ( 'NONE', ( #3947, #1847, #2985, #1194 ) ) ;
#399 = COLOUR_RGB ( '',0.8941176470588234615, 0.8941176470588234615, 0.8941176470588234615 ) ;
#400 = AXIS2_PLACEMENT_3D ( 'NONE', #2687, #1043, #599 ) ;
#401 =( GEOMETRIC_REPRESENTATION_CONTEXT ( 3 ) GLOBAL_UNCERTAINTY_ASSIGNED_CONTEXT ( ( #3253 ) ) GLOBAL_UNIT_ASSIGNED_CONTEXT ( ( #4, #2110, #4596 ) ) REPRESENTATION_CONTEXT ( 'NONE', 'WORKASPACE' ) );
#402 = CARTESIAN_POINT ( 'NONE',  ( 0.000000000000000000, 0.000000000000000000, -11.97459999999999880 ) ) ;
#403 = B_SPLINE_CURVE_WITH_KNOTS ( 'NONE', 3,
 ( #411, #4225, #176, #667, #3919, #915, #1835, #3946, #2719 ),
 .UNSPECIFIED., .F., .F.,
 ( 4, 2, 1, 2, 4 ),
 ( 0.000000000000000000, 0.002598076211353316737, 0.005196152422706633474, 0.007794228634059948910, 0.01039230484541326521 ),
 .UNSPECIFIED. ) ;
#404 = ORIENTED_EDGE ( 'NONE', *, *, #632, .T. ) ;
#405 = MECHANICAL_DESIGN_GEOMETRIC_PRESENTATION_REPRESENTATION (  '', ( #1277 ), #227 ) ;
#406 = ORIENTED_EDGE ( 'NONE', *, *, #1500, .F. ) ;
#407 = ADVANCED_FACE ( 'NONE', ( #828 ), #1256, .T. ) ;
#408 = ADVANCED_FACE ( 'NONE', ( #4526 ), #855, .T. ) ;
#409 = ORIENTED_EDGE ( 'NONE', *, *, #3431, .T. ) ;
#410 = CYLINDRICAL_SURFACE ( 'NONE', #2644, 15.00000000000000000 ) ;
#411 = CARTESIAN_POINT ( 'NONE',  ( 9.000000000000000000, 5.196152422706629359, -8.935996291721334472 ) ) ;
#412 = CARTESIAN_POINT ( 'NONE',  ( 9.506737344437272696, 5.488717364925924436, -9.686084310752812954 ) ) ;
#413 = DIRECTION ( 'NONE',  ( 0.000000000000000000, 0.000000000000000000, 1.000000000000000000 ) ) ;
#414 = ITEM_DEFINED_TRANSFORMATION ( 'NONE', 'NONE', #662,  #4154 ) ;
#415 = CONICAL_SURFACE ( 'NONE', #4083, 12.38940648156203927, 1.221730476396048370 ) ;
#416 = B_SPLINE_CURVE_WITH_KNOTS ( 'NONE', 3,
 ( #185, #4385, #3497, #1797, #3906, #3060, #5151, #4699, #2649 ),
 .UNSPECIFIED., .F., .F.,
 ( 4, 2, 1, 2, 4 ),
 ( 0.000000000000000000, 0.002598076211353316737, 0.005196152422706633474, 0.007794228634059951512, 0.01039230484541326521 ),
 .UNSPECIFIED. ) ;
#417 = ORIENTED_EDGE ( 'NONE', *, *, #3310, .F. ) ;
#418 = CARTESIAN_POINT ( 'NONE',  ( 0.000000000000000000, -5.839897972853064445, 4.770489558936219510E-15 ) ) ;
#419 = SURFACE_STYLE_USAGE ( .BOTH. , #2470 ) ;
#420 = AXIS2_PLACEMENT_3D ( 'NONE', #4558, #2003, #4859 ) ;
#421 = CARTESIAN_POINT ( 'NONE',  ( 92.00000000000000000, 0.000000000000000000, 0.000000000000000000 ) ) ;
#422 = CARTESIAN_POINT ( 'NONE',  ( 4.500000000000001776, -7.794228634059955141, -8.419403919045802098 ) ) ;
#423 = AXIS2_PLACEMENT_3D ( 'NONE', #2818, #3697, #3285 ) ;
#424 = ORIENTED_EDGE ( 'NONE', *, *, #507, .T. ) ;
#425 = CARTESIAN_POINT ( 'NONE',  ( 9.058808647644763568, 5.230105611255011944, -9.269271692759767589 ) ) ;
#426 = CARTESIAN_POINT ( 'NONE',  ( 9.000000000000000000, 0.2246546977803023648, 1.531435568635775407E-15 ) ) ;
#427 = ORIENTED_EDGE ( 'NONE', *, *, #4247, .F. ) ;
#428 = VERTEX_POINT ( 'NONE', #361 ) ;
#429 = DIRECTION ( 'NONE',  ( 1.000000000000000000, -0.000000000000000000, -0.000000000000000000 ) ) ;
#430 = ORIENTED_EDGE ( 'NONE', *, *, #862, .F. ) ;
#431 =( LENGTH_UNIT ( ) NAMED_UNIT ( * ) SI_UNIT ( .MILLI., .METRE. ) );
#432 = VERTEX_POINT ( 'NONE', #439 ) ;
#433 = EDGE_CURVE ( 'NONE', #752, #1641, #4908, .T. ) ;
#434 = CARTESIAN_POINT ( 'NONE',  ( -25.00000000000000000, 60.00000000000000711, 25.00000000000000000 ) ) ;
#435 = EDGE_CURVE ( 'NONE', #3050, #273, #1180, .T. ) ;
#436 = CARTESIAN_POINT ( 'NONE',  ( -150.0000000000000000, 870.0000000000000000, -5.999999999999950262 ) ) ;
#437 = CARTESIAN_POINT ( 'NONE',  ( -5.284168072928043358, -7.341488986065035860, -3.941244303574257900E-15 ) ) ;
#438 = PLANE ( 'NONE',  #3355 ) ;
#439 = CARTESIAN_POINT ( 'NONE',  ( -74.99999999999998579, 582.4999999999997726, 49.99999999999998579 ) ) ;
#440 = CARTESIAN_POINT ( 'NONE',  ( -1.447884101293563486, -9.556368569776052979, -0.5428950306860302888 ) ) ;
#441 = CARTESIAN_POINT ( 'NONE',  ( -1.676835913137321903E-15, 35.00000000000000000, -25.00000000000000000 ) ) ;
#442 = DIRECTION ( 'NONE',  ( 1.000000000000000000, 0.000000000000000000, 1.850371707708594316E-16 ) ) ;
#443 = PRODUCT ( 'support yoke', 'support yoke', '', ( #4465 ) ) ;
#444 = ORIENTED_EDGE ( 'NONE', *, *, #762, .T. ) ;
#445 = ORIENTED_EDGE ( 'NONE', *, *, #3007, .T. ) ;
#446 = CARTESIAN_POINT ( 'NONE',  ( -0.3349232592648703211, 10.58567287930770817, -9.544071379897774321 ) ) ;
#447 = CARTESIAN_POINT ( 'NONE',  ( 9.000000000000001776, 0.9001646245238089650, -0.03631462189738251384 ) ) ;
#448 = ORIENTED_EDGE ( 'NONE', *, *, #1572, .F. ) ;
#449 = ORIENTED_EDGE ( 'NONE', *, *, #2982, .F. ) ;
#450 =( GEOMETRIC_REPRESENTATION_CONTEXT ( 3 ) GLOBAL_UNCERTAINTY_ASSIGNED_CONTEXT ( ( #3198 ) ) GLOBAL_UNIT_ASSIGNED_CONTEXT ( ( #3688, #4189, #3379 ) ) REPRESENTATION_CONTEXT ( 'NONE', 'WORKASPACE' ) );
#451 = ORIENTED_EDGE ( 'NONE', *, *, #2561, .F. ) ;
#452 = ADVANCED_FACE ( 'NONE', ( #3291 ), #4007, .T. ) ;
#453 = EDGE_CURVE ( 'NONE', #5233, #1447, #4280, .T. ) ;
#454 = DIRECTION ( 'NONE',  ( -1.000000000000000000, 0.000000000000000000, 0.000000000000000000 ) ) ;
#455 = ORIENTED_EDGE ( 'NONE', *, *, #4975, .F. ) ;
#456 =( NAMED_UNIT ( * ) SI_UNIT ( $, .STERADIAN. ) SOLID_ANGLE_UNIT ( ) );
#457 = VERTEX_POINT ( 'NONE', #162 ) ;
#458 = EDGE_CURVE ( 'NONE', #3578, #4918, #3803, .T. ) ;
#459 = DIRECTION ( 'NONE',  ( 0.000000000000000000, -1.000000000000000000, 0.000000000000000000 ) ) ;
#460 = CARTESIAN_POINT ( 'NONE',  ( -6.134460314789387247, 6.850572531336530879, -8.512883888440001101 ) ) ;
#461 = FACE_OUTER_BOUND ( 'NONE', #710, .T. ) ;
#462 = PLANE ( 'NONE',  #2932 ) ;
#463 = LINE ( 'NONE', #132, #3357 ) ;
#464 = FILL_AREA_STYLE ('',( #3292 ) ) ;
#465 = CARTESIAN_POINT ( 'NONE',  ( 0.000000000000000000, 2.919948986426526005, -5.057500000000002771 ) ) ;
#466 = CARTESIAN_POINT ( 'NONE',  ( -8.999999999999996447, -5.582885416786369071, -9.544070791154714684 ) ) ;
#467 = B_SPLINE_CURVE_WITH_KNOTS ( 'NONE', 3,
 ( #4058, #658, #2326, #3615, #5307, #3231, #340, #4002, #252, #2770 ),
 .UNSPECIFIED., .F., .F.,
 ( 4, 2, 2, 2, 4 ),
 ( 0.000000000000000000, 0.002766603965071789267, 0.005533207930143578535, 0.008299811895215367802, 0.01106641586028715707 ),
 .UNSPECIFIED. ) ;
#468 = CIRCLE ( 'NONE', #3263, 15.00000000000000000 ) ;
#469 = SURFACE_STYLE_USAGE ( .BOTH. , #4208 ) ;
#470 = EDGE_CURVE ( 'NONE', #4891, #4946, #540, .T. ) ;
#471 = ADVANCED_FACE ( 'NONE', ( #519 ), #2233, .F. ) ;
#472 = VECTOR ( 'NONE', #3512, 1000.000000000000000 ) ;
#473 = EDGE_CURVE ( 'NONE', #2752, #4279, #2547, .T. ) ;
#474 = ORIENTED_EDGE ( 'NONE', *, *, #2211, .F. ) ;
#475 = LINE ( 'NONE', #2130, #5231 ) ;
#476 = CARTESIAN_POINT ( 'NONE',  ( 9.416515850482076289, 4.955676884309055730, -9.021433408186453562 ) ) ;
#477 = UNCERTAINTY_MEASURE_WITH_UNIT (LENGTH_MEASURE( 1.000000000000000082E-05 ), #4680, 'distance_accuracy_value', 'NONE');
#478 = CARTESIAN_POINT ( 'NONE',  ( 9.000000000000001776, 4.786605659887718467, -1.023509873932519687 ) ) ;
#479 = ORIENTED_EDGE ( 'NONE', *, *, #5292, .T. ) ;
#480 = AXIS2_PLACEMENT_3D ( 'NONE', #2323, #4390, #2713 ) ;
#481 = AXIS2_PLACEMENT_3D ( 'NONE', #1, #2031, #1622 ) ;
#482 = CARTESIAN_POINT ( 'NONE',  ( 0.000000000000000000, 0.000000000000000000, -10.20000000000000107 ) ) ;
#483 = PRODUCT_DEFINITION_FORMATION_WITH_SPECIFIED_SOURCE ( 'ANY', '', #4971, .NOT_KNOWN. ) ;
#484 = AXIS2_PLACEMENT_3D ( 'NONE', #2475, #4889, #2828 ) ;
#485 =( GEOMETRIC_REPRESENTATION_CONTEXT ( 3 ) GLOBAL_UNCERTAINTY_ASSIGNED_CONTEXT ( ( #3762 ) ) GLOBAL_UNIT_ASSIGNED_CONTEXT ( ( #4296, #3410, #1343 ) ) REPRESENTATION_CONTEXT ( 'NONE', 'WORKASPACE' ) );
#486 = EDGE_LOOP ( 'NONE', ( #2087, #1135, #1675, #1922 ) ) ;
#487 = DIRECTION ( 'NONE',  ( 0.000000000000000000, 0.000000000000000000, 1.000000000000000000 ) ) ;
#488 = AXIS2_PLACEMENT_3D ( 'NONE', #3147, #2245, #5188 ) ;
#489 = DIRECTION ( 'NONE',  ( 1.000000000000000000, 0.000000000000000000, 0.000000000000000000 ) ) ;
#490 = CARTESIAN_POINT ( 'NONE',  ( -5.287803175666994981, 7.339390258519110866, -8.964894084809513330 ) ) ;
#491 = STYLED_ITEM ( 'NONE', ( #4235 ), #1615 ) ;
#492 = CARTESIAN_POINT ( 'NONE',  ( 2.822677224501522808, -8.762631390014002264, -8.969375302469423161 ) ) ;
#493 = PRODUCT_DEFINITION_SHAPE ( 'NONE', 'NONE',  #3566 ) ;
#494 = VECTOR ( 'NONE', #4759, 1000.000000000000000 ) ;
#495 = PRESENTATION_LAYER_ASSIGNMENT (  '', '', ( #3380 ) ) ;
#496 = FACE_BOUND ( 'NONE', #2841, .T. ) ;
#497 = DIRECTION ( 'NONE',  ( 0.000000000000000000, 0.000000000000000000, -1.000000000000000000 ) ) ;
#498 = CARTESIAN_POINT ( 'NONE',  ( 6.000000000000000000, 0.000000000000000000, 0.000000000000000000 ) ) ;
#499 = CARTESIAN_POINT ( 'NONE',  ( -9.000000000000000000, 5.677108048117061045, -9.021434243155090016 ) ) ;
#500 =( NAMED_UNIT ( * ) SI_UNIT ( $, .STERADIAN. ) SOLID_ANGLE_UNIT ( ) );
#501 = APPLICATION_CONTEXT ( 'automotive_design' ) ;
#502 = AXIS2_PLACEMENT_3D ( 'NONE', #1265, #2612, #74 ) ;
#503 = VERTEX_POINT ( 'NONE', #879 ) ;
#504 = FILL_AREA_STYLE_COLOUR ( '', #807 ) ;
#505 = DIRECTION ( 'NONE',  ( -0.000000000000000000, -0.000000000000000000, 1.000000000000000000 ) ) ;
#506 = CARTESIAN_POINT ( 'NONE',  ( 0.000000000000000000, 0.000000000000000000, -0.6301867843887398735 ) ) ;
#507 = EDGE_CURVE ( 'NONE', #2252, #1603, #88, .T. ) ;
#508 = VERTEX_POINT ( 'NONE', #3877 ) ;
#509 = CIRCLE ( 'NONE', #2248, 6.499999999999999112 ) ;
#510 = DIRECTION ( 'NONE',  ( -0.000000000000000000, -0.000000000000000000, 1.000000000000000000 ) ) ;
#511 =( BOUNDED_SURFACE ( )  B_SPLINE_SURFACE ( 3, 2, ( 
 ( #499, #2943, #860 ),
 ( #1240, #1726, #5052 ),
 ( #2101, #1290, #1311 ),
 ( #2159, #3857, #2499 ),
 ( #4628, #3833, #4581 ),
 ( #2081, #2919, #2991 ),
 ( #1332, #3779, #2528 ),
 ( #899, #466, #5078 ) ),
 .UNSPECIFIED., .F., .F., .F. ) 
 B_SPLINE_SURFACE_WITH_KNOTS ( ( 4, 2, 2, 4 ),
 ( 3, 3 ),
 ( 0.04601127232121990374, 0.05157242366991564297, 0.05435299934426351259, 0.05713357501861138221 ),
 ( 0.000000000000000000, 1.000000000000000000 ),
 .UNSPECIFIED. ) 
 GEOMETRIC_REPRESENTATION_ITEM ( )  RATIONAL_B_SPLINE_SURFACE ( (
 ( 1.000000000000000000, 0.8047781497997479327, 1.000000000000000000),
 ( 1.000000000000000000, 0.8123770896799767938, 1.000000000000000000),
 ( 1.000000000000000000, 0.8190668965778666877, 1.000000000000000000),
 ( 1.000000000000000000, 0.8191933289379096372, 1.000000000000000000),
 ( 1.000000000000000000, 0.8176087259132261975, 1.000000000000000000),
 ( 1.000000000000000000, 0.8122957709810018079, 1.000000000000000000),
 ( 1.000000000000000000, 0.8086309318960932524, 1.000000000000000000),
 ( 1.000000000000000000, 0.8047712439490427583, 1.000000000000000000) ) ) 
 REPRESENTATION_ITEM ( '' )  SURFACE ( )  );
#512 = ORIENTED_EDGE ( 'NONE', *, *, #139, .F. ) ;
#513 = DIRECTION ( 'NONE',  ( -1.000000000000000000, 1.224646799147352468E-16, 0.000000000000000000 ) ) ;
#514 = EDGE_LOOP ( 'NONE', ( #1436, #4747, #4585, #3936, #2557 ) ) ;
#515 = CARTESIAN_POINT ( 'NONE',  ( 0.000000000000000000, 840.0000000000001137, 0.000000000000000000 ) ) ;
#516 = DIRECTION ( 'NONE',  ( -0.000000000000000000, -1.000000000000000000, -0.000000000000000000 ) ) ;
#517 = EDGE_CURVE ( 'NONE', #5301, #3270, #463, .T. ) ;
#518 = DIRECTION ( 'NONE',  ( 0.000000000000000000, 0.000000000000000000, -1.000000000000000000 ) ) ;
#519 = FACE_OUTER_BOUND ( 'NONE', #1880, .T. ) ;
#520 = CARTESIAN_POINT ( 'NONE',  ( 121.7157287525372311, -20.00000000000000000, -106.7157287525388369 ) ) ;
#521 = EDGE_CURVE ( 'NONE', #1452, #4077, #3495, .T. ) ;
#522 = LINE ( 'NONE', #1310, #5104 ) ;
#523 = LINE ( 'NONE', #3324, #777 ) ;
#524 = FILL_AREA_STYLE ('',( #951 ) ) ;
#525 = ORIENTED_EDGE ( 'NONE', *, *, #1984, .T. ) ;
#526 = CARTESIAN_POINT ( 'NONE',  ( 121.7157287525384533, -20.00000000000000000, 106.7157287525376859 ) ) ;
#527 = CARTESIAN_POINT ( 'NONE',  ( 0.3968280142506481756, 10.16319608456367085, -8.848996304171389937 ) ) ;
#528 = CARTESIAN_POINT ( 'NONE',  ( -24.99999999999999645, 610.0000000000000000, -25.00000000000000000 ) ) ;
#529 = VERTEX_POINT ( 'NONE', #4604 ) ;
#530 = VECTOR ( 'NONE', #4346, 1000.000000000000000 ) ;
#531 = EDGE_CURVE ( 'NONE', #1147, #207, #4577, .T. ) ;
#532 = CARTESIAN_POINT ( 'NONE',  ( 6.430436718082018110, -6.679690475221758739, -0.2264046624879813563 ) ) ;
#533 = EDGE_CURVE ( 'NONE', #432, #3578, #4203, .T. ) ;
#534 = EDGE_LOOP ( 'NONE', ( #2806, #1893, #3164, #1680 ) ) ;
#535 = EDGE_CURVE ( 'NONE', #4624, #5043, #1720, .T. ) ;
#536 = DIRECTION ( 'NONE',  ( -0.000000000000000000, -0.000000000000000000, 1.000000000000000000 ) ) ;
#537 = CARTESIAN_POINT ( 'NONE',  ( -25.00000000000000000, 10.00000000000000000, 25.00000000000000000 ) ) ;
#538 = DIRECTION ( 'NONE',  ( 1.000000000000000000, 0.000000000000000000, 0.000000000000000000 ) ) ;
#539 = VERTEX_POINT ( 'NONE', #3009 ) ;
#540 = LINE ( 'NONE', #569, #3063 ) ;
#541 = CARTESIAN_POINT ( 'NONE',  ( 0.000000000000000000, 0.000000000000000000, 0.000000000000000000 ) ) ;
#542 = DIRECTION ( 'NONE',  ( 0.000000000000000000, 0.000000000000000000, -1.000000000000000000 ) ) ;
#543 = ADVANCED_FACE ( 'NONE', ( #3473 ), #4262, .F. ) ;
#544 = FACE_BOUND ( 'NONE', #1003, .T. ) ;
#545 = DIRECTION ( 'NONE',  ( 1.000000000000000000, 0.000000000000000000, 0.000000000000000000 ) ) ;
#546 = CARTESIAN_POINT ( 'NONE',  ( 3.715831927071962859, -8.246968282054865540, -4.078463641029454555E-15 ) ) ;
#547 = ORIENTED_EDGE ( 'NONE', *, *, #2794, .F. ) ;
#548 = DIRECTION ( 'NONE',  ( 0.000000000000000000, -0.5000000000000012212, -0.8660254037844380415 ) ) ;
#549 = CARTESIAN_POINT ( 'NONE',  ( 1.447884101293554382, 9.556368569776049426, -0.5428950306860281794 ) ) ;
#550 = LINE ( 'NONE', #4527, #3102 ) ;
#551 = CYLINDRICAL_SURFACE ( 'NONE', #3899, 15.00000000000000000 ) ;
#552 = AXIS2_PLACEMENT_3D ( 'NONE', #2520, #375, #1596 ) ;
#553 = ADVANCED_FACE ( 'NONE', ( #3829 ), #1254, .T. ) ;
#554 = CARTESIAN_POINT ( 'NONE',  ( -1.676835913137321903E-15, 35.00000000000000000, 30.00000000000000711 ) ) ;
#555 = CIRCLE ( 'NONE', #1685, 6.499999999999983125 ) ;
#556 = PRESENTATION_STYLE_ASSIGNMENT (( #4250 ) ) ;
#557 = VECTOR ( 'NONE', #1931, 1000.000000000000000 ) ;
#558 = ORIENTED_EDGE ( 'NONE', *, *, #3838, .F. ) ;
#559 = CARTESIAN_POINT ( 'NONE',  ( 6.000000000000000000, -2.919948986426526893, 5.057500000000001883 ) ) ;
#560 = DIRECTION ( 'NONE',  ( 0.000000000000000000, 0.000000000000000000, 1.000000000000000000 ) ) ;
#561 = CARTESIAN_POINT ( 'NONE',  ( -6.000000000000000888, 7.347880794884120722E-16, -12.00000000000000000 ) ) ;
#562 = VECTOR ( 'NONE', #3463, 1000.000000000000000 ) ;
#563 = EDGE_CURVE ( 'NONE', #3747, #5361, #2873, .T. ) ;
#564 = EDGE_CURVE ( 'NONE', #1204, #676, #3614, .T. ) ;
#565 = PRODUCT_DEFINITION_FORMATION_WITH_SPECIFIED_SOURCE ( 'ANY', '', #313, .NOT_KNOWN. ) ;
#566 = AXIS2_PLACEMENT_3D ( 'NONE', #1191, #724, #3740 ) ;
#567 = ORIENTED_EDGE ( 'NONE', *, *, #1362, .T. ) ;
#568 = ORIENTED_EDGE ( 'NONE', *, *, #2743, .T. ) ;
#569 = CARTESIAN_POINT ( 'NONE',  ( 1.410908427127813464E-14, 582.4999999999997726, 30.00000000000000711 ) ) ;
#570 = CARTESIAN_POINT ( 'NONE',  ( -150.0000000000000000, 810.0000000000000000, -25.00000000000000000 ) ) ;
#571 = LINE ( 'NONE', #2235, #3982 ) ;
#572 = EDGE_LOOP ( 'NONE', ( #2231, #4802, #4354, #3593 ) ) ;
#573 = CARTESIAN_POINT ( 'NONE',  ( 0.000000000000000000, 840.0000000000001137, 0.000000000000000000 ) ) ;
#574 = DIRECTION ( 'NONE',  ( 1.000000000000000000, 0.000000000000000000, 0.000000000000000000 ) ) ;
#575 = AXIS2_PLACEMENT_3D ( 'NONE', #2584, #3757, #4233 ) ;
#576 = PRODUCT_DEFINITION_SHAPE ( 'NONE', 'NONE',  #5391 ) ;
#577 = EDGE_LOOP ( 'NONE', ( #3215, #4979 ) ) ;
#578 = LINE ( 'NONE', #4762, #3087 ) ;
#579 = ORIENTED_EDGE ( 'NONE', *, *, #4487, .F. ) ;
#580 = CARTESIAN_POINT ( 'NONE',  ( 137.5000000000000000, 870.0000000000000000, 0.000000000000000000 ) ) ;
#581 = LINE ( 'NONE', #1466, #1103 ) ;
#582 = CARTESIAN_POINT ( 'NONE',  ( -6.499999999999988454, 330.0000000000000000, 25.00000000000000000 ) ) ;
#583 = CARTESIAN_POINT ( 'NONE',  ( 7.960204194457795477E-16, 810.0000000000000000, -6.499999999999999112 ) ) ;
#584 = VECTOR ( 'NONE', #1682, 1000.000000000000000 ) ;
#585 = CARTESIAN_POINT ( 'NONE',  ( -31.74999999999995737, 0.000000000000000000, 0.000000000000000000 ) ) ;
#586 = LINE ( 'NONE', #5193, #5037 ) ;
#587 = PRODUCT_RELATED_PRODUCT_CATEGORY ( 'part', '', ( #976 ) ) ;
#588 = VECTOR ( 'NONE', #5212, 1000.000000000000000 ) ;
#589 = ORIENTED_EDGE ( 'NONE', *, *, #453, .T. ) ;
#590 = FILL_AREA_STYLE_COLOUR ( '', #205 ) ;
#591 = CARTESIAN_POINT ( 'NONE',  ( 0.000000000000000000, 570.0000000000000000, 25.00000000000000000 ) ) ;
#592 = LINE ( 'NONE', #537, #4258 ) ;
#593 = EDGE_CURVE ( 'NONE', #285, #2404, #4298, .T. ) ;
#594 = ORIENTED_EDGE ( 'NONE', *, *, #829, .T. ) ;
#595 = ORIENTED_EDGE ( 'NONE', *, *, #3799, .F. ) ;
#596 = DIRECTION ( 'NONE',  ( 0.000000000000000000, -1.000000000000000000, 0.000000000000000000 ) ) ;
#597 = PLANE ( 'NONE',  #2591 ) ;
#598 = CARTESIAN_POINT ( 'NONE',  ( 121.7157287525384533, -20.00000000000000000, 106.7157287525376859 ) ) ;
#599 = DIRECTION ( 'NONE',  ( 0.000000000000000000, 0.000000000000000000, 1.000000000000000000 ) ) ;
#600 = DIRECTION ( 'NONE',  ( -0.000000000000000000, -0.000000000000000000, 1.000000000000000000 ) ) ;
#601 = VERTEX_POINT ( 'NONE', #2623 ) ;
#602 = PLANE ( 'NONE',  #2186 ) ;
#603 = CARTESIAN_POINT ( 'NONE',  ( 25.00000000000000355, 60.00000000000000711, 25.00000000000000000 ) ) ;
#604 = CARTESIAN_POINT ( 'NONE',  ( 0.000000000000000000, 0.000000000000000000, -11.97459999999999880 ) ) ;
#605 = CARTESIAN_POINT ( 'NONE',  ( 6.000000000000000000, -2.919948986426539772, -5.057499999999996554 ) ) ;
#606 = CARTESIAN_POINT ( 'NONE',  ( 9.000000000000000000, -5.677101382972238319, -9.021433019664915065 ) ) ;
#607 = CARTESIAN_POINT ( 'NONE',  ( 12.59999999999999964, 0.000000000000000000, -6.600000000000001421 ) ) ;
#608 = ORIENTED_EDGE ( 'NONE', *, *, #458, .F. ) ;
#609 = EDGE_CURVE ( 'NONE', #1113, #3556, #5351, .T. ) ;
#610 = EDGE_LOOP ( 'NONE', ( #4702, #3435, #2634, #3659 ) ) ;
#611 = EDGE_CURVE ( 'NONE', #4353, #4532, #731, .T. ) ;
#612 = EDGE_CURVE ( 'NONE', #3569, #2957, #2707, .T. ) ;
#613 = EDGE_LOOP ( 'NONE', ( #1737, #3788, #3192, #3312 ) ) ;
#614 = CARTESIAN_POINT ( 'NONE',  ( -9.497968775322179980, -4.580952057516538112, -9.518120616476199558 ) ) ;
#615 = EDGE_LOOP ( 'NONE', ( #2413, #3333, #5322, #568 ) ) ;
#616 = CARTESIAN_POINT ( 'NONE',  ( 91.03600000000004400, 7.347880794884120722E-16, -6.000000000000000888 ) ) ;
#617 = DIRECTION ( 'NONE',  ( 0.000000000000000000, 0.000000000000000000, -1.000000000000000000 ) ) ;
#618 = ADVANCED_FACE ( 'NONE', ( #2787 ), #1458, .T. ) ;
#619 = ORIENTED_EDGE ( 'NONE', *, *, #1469, .F. ) ;
#620 = CARTESIAN_POINT ( 'NONE',  ( 9.000000000000000000, 5.196152422706629359, -12.00000000000000000 ) ) ;
#621 = DIRECTION ( 'NONE',  ( 1.000000000000000000, 0.000000000000000000, -0.000000000000000000 ) ) ;
#622 = CARTESIAN_POINT ( 'NONE',  ( 0.000000000000000000, 0.000000000000000000, -25.03750572909317285 ) ) ;
#623 = DIRECTION ( 'NONE',  ( -1.000000000000000000, -0.000000000000000000, -0.000000000000000000 ) ) ;
#624 =( NAMED_UNIT ( * ) SI_UNIT ( $, .STERADIAN. ) SOLID_ANGLE_UNIT ( ) );
#625 = ORIENTED_EDGE ( 'NONE', *, *, #691, .T. ) ;
#626 = CARTESIAN_POINT ( 'NONE',  ( 9.000000000000001776, -4.785828667975444262, -1.023175036954118378 ) ) ;
#627 = CARTESIAN_POINT ( 'NONE',  ( -9.506737344437272696, -5.488717364925931541, -9.686084310752812954 ) ) ;
#628 = CARTESIAN_POINT ( 'NONE',  ( 6.000000000000000000, 7.347880794884119736E-16, -11.97459999999999880 ) ) ;
#629 = DIRECTION ( 'NONE',  ( -0.000000000000000000, -0.000000000000000000, 1.000000000000000000 ) ) ;
#630 = CARTESIAN_POINT ( 'NONE',  ( 0.6000000000000033085, 1.102182119232617714E-15, -9.000000000000000000 ) ) ;
#631 = EDGE_CURVE ( 'NONE', #4555, #366, #3353, .T. ) ;
#632 = EDGE_CURVE ( 'NONE', #4595, #4480, #646, .T. ) ;
#633 = CARTESIAN_POINT ( 'NONE',  ( 9.000000000000000000, 0.9268837573866910429, -8.460786308154190749 ) ) ;
#634 = FACE_OUTER_BOUND ( 'NONE', #1339, .T. ) ;
#635 = ORIENTED_EDGE ( 'NONE', *, *, #2387, .T. ) ;
#636 = AXIS2_PLACEMENT_3D ( 'NONE', #2673, #4331, #1507 ) ;
#637 = EDGE_LOOP ( 'NONE', ( #743, #2019, #3494, #1929 ) ) ;
#638 = DIRECTION ( 'NONE',  ( 0.000000000000000000, 0.000000000000000000, 1.000000000000000000 ) ) ;
#639 = ORIENTED_EDGE ( 'NONE', *, *, #709, .F. ) ;
#640 = DIRECTION ( 'NONE',  ( -0.000000000000000000, -0.000000000000000000, 1.000000000000000000 ) ) ;
#641 = COLOUR_RGB ( '',0.8941176470588234615, 0.8941176470588234615, 0.8941176470588234615 ) ;
#642 =( BOUNDED_SURFACE ( )  B_SPLINE_SURFACE ( 3, 2, ( 
 ( #3137, #4384, #3580 ),
 ( #2317, #3990, #1119 ),
 ( #1173, #244, #1950 ),
 ( #3642, #3607, #2788 ),
 ( #3194, #2348, #2848 ),
 ( #1459, #3695, #4812 ),
 ( #4046, #1144, #2014 ),
 ( #5236, #2374, #712 ) ),
 .UNSPECIFIED., .F., .F., .T. ) 
 B_SPLINE_SURFACE_WITH_KNOTS ( ( 4, 2, 2, 4 ),
 ( 3, 3 ),
 ( 0.04613854442509286724, 0.05169925677048781143, 0.05447961294318528352, 0.05725996911588275562 ),
 ( 0.000000000000000000, 1.000000000000000000 ),
 .UNSPECIFIED. ) 
 GEOMETRIC_REPRESENTATION_ITEM ( )  RATIONAL_B_SPLINE_SURFACE ( (
 ( 1.000000000000000000, 0.8047781684971936356, 1.000000000000000000),
 ( 1.000000000000000000, 0.8123765127741280345, 1.000000000000000000),
 ( 1.000000000000000000, 0.8190661184402779904, 1.000000000000000000),
 ( 1.000000000000000000, 0.8191936944251213548, 1.000000000000000000),
 ( 1.000000000000000000, 0.8176092056339585579, 1.000000000000000000),
 ( 1.000000000000000000, 0.8122961334886904528, 1.000000000000000000),
 ( 1.000000000000000000, 0.8086310951057483765, 1.000000000000000000),
 ( 1.000000000000000000, 0.8047712311394934481, 1.000000000000000000) ) ) 
 REPRESENTATION_ITEM ( '' )  SURFACE ( )  );
#643 = ORIENTED_EDGE ( 'NONE', *, *, #4196, .T. ) ;
#644 = AXIS2_PLACEMENT_3D ( 'NONE', #1226, #3354, #2903 ) ;
#645 = ORIENTED_EDGE ( 'NONE', *, *, #531, .T. ) ;
#646 = LINE ( 'NONE', #1398, #2482 ) ;
#647 = CARTESIAN_POINT ( 'NONE',  ( 6.048361762532168839, 6.900281553659078249, -0.1192015822679150933 ) ) ;
#648 = DIRECTION ( 'NONE',  ( -0.000000000000000000, -0.000000000000000000, 1.000000000000000000 ) ) ;
#649 = DIRECTION ( 'NONE',  ( 1.000000000000000000, 0.000000000000000000, -0.000000000000000000 ) ) ;
#650 = FILL_AREA_STYLE_COLOUR ( '', #1426 ) ;
#651 = PRODUCT_RELATED_PRODUCT_CATEGORY ( 'part', '', ( #443 ) ) ;
#652 = VECTOR ( 'NONE', #4092, 1000.000000000000000 ) ;
#653 = COLOUR_RGB ( '',0.8941176470588234615, 0.8941176470588234615, 0.8941176470588234615 ) ;
#654 = ORIENTED_EDGE ( 'NONE', *, *, #80, .T. ) ;
#655 = CARTESIAN_POINT ( 'NONE',  ( -1.301042606982605321E-14, -10.39230484541326760, -1.199999999999999734 ) ) ;
#656 = VERTEX_POINT ( 'NONE', #3193 ) ;
#657 = DIRECTION ( 'NONE',  ( 1.000000000000000000, 0.000000000000000000, 0.000000000000000000 ) ) ;
#658 = CARTESIAN_POINT ( 'NONE',  ( -8.716942385998455833, 5.934590066575458955, -9.518277236634762772 ) ) ;
#659 = CARTESIAN_POINT ( 'NONE',  ( -24.99999999999999645, 610.0000000000000000, -25.00000000000000000 ) ) ;
#660 = CARTESIAN_POINT ( 'NONE',  ( 0.000000000000000000, 0.000000000000000000, 0.000000000000000000 ) ) ;
#661 = AXIS2_PLACEMENT_3D ( 'NONE', #1997, #4504, #3704 ) ;
#662 = AXIS2_PLACEMENT_3D ( 'NONE', #977, #3117, #574 ) ;
#663 = VECTOR ( 'NONE', #4725, 1000.000000000000000 ) ;
#664 =( GEOMETRIC_REPRESENTATION_CONTEXT ( 3 ) GLOBAL_UNCERTAINTY_ASSIGNED_CONTEXT ( ( #4876 ) ) GLOBAL_UNIT_ASSIGNED_CONTEXT ( ( #2048, #3372, #4579 ) ) REPRESENTATION_CONTEXT ( 'NONE', 'WORKASPACE' ) );
#665 = EDGE_CURVE ( 'NONE', #5319, #2146, #4998, .T. ) ;
#666 = CARTESIAN_POINT ( 'NONE',  ( 9.473646573774082924, 0.9034019355243676497, -9.137364994939673579 ) ) ;
#667 = CARTESIAN_POINT ( 'NONE',  ( 5.999999999999999112, 6.928203230275508773, -8.505011083697292307 ) ) ;
#668 = EDGE_LOOP ( 'NONE', ( #567, #1976, #3304, #3651 ) ) ;
#669 =( LENGTH_UNIT ( ) NAMED_UNIT ( * ) SI_UNIT ( .MILLI., .METRE. ) );
#670 = AXIS2_PLACEMENT_3D ( 'NONE', #4308, #1005, #621 ) ;
#671 = ORIENTED_EDGE ( 'NONE', *, *, #1136, .T. ) ;
#672 =( REPRESENTATION_RELATIONSHIP ('NONE','NONE', #4791, #1065 ) REPRESENTATION_RELATIONSHIP_WITH_TRANSFORMATION ( #778 )SHAPE_REPRESENTATION_RELATIONSHIP( ) );
#673 = AXIS2_PLACEMENT_3D ( 'NONE', #2773, #341, #4135 ) ;
#674 = EDGE_LOOP ( 'NONE', ( #474, #4449, #1677, #4999 ) ) ;
#675 = DIRECTION ( 'NONE',  ( 0.000000000000000000, -0.7071067811865765496, -0.7071067811865185959 ) ) ;
#676 = VERTEX_POINT ( 'NONE', #2760 ) ;
#677 = CARTESIAN_POINT ( 'NONE',  ( -150.0000000000000000, 810.0000000000000000, 25.00000000000000000 ) ) ;
#678 = DIRECTION ( 'NONE',  ( 0.000000000000000000, 0.000000000000000000, -1.000000000000000000 ) ) ;
#679 = AXIS2_PLACEMENT_3D ( 'NONE', #2078, #13, #3676 ) ;
#680 = VECTOR ( 'NONE', #5152, 1000.000000000000000 ) ;
#681 = ORIENTED_EDGE ( 'NONE', *, *, #2414, .T. ) ;
#682 = EDGE_LOOP ( 'NONE', ( #4010, #1247, #200, #1167 ) ) ;
#683 = CARTESIAN_POINT ( 'NONE',  ( -5.284395884496540852, 7.341357458994635543, -0.03002505116509866095 ) ) ;
#684 = CARTESIAN_POINT ( 'NONE',  ( -30.00000000000000000, 610.0000000000000000, -30.00000000000000355 ) ) ;
#685 = CARTESIAN_POINT ( 'NONE',  ( 0.000000000000000000, 0.000000000000000000, 0.000000000000000000 ) ) ;
#686 = CARTESIAN_POINT ( 'NONE',  ( 150.0000000000000000, 885.0000000000000000, -25.00000000000000000 ) ) ;
#687 = ITEM_DEFINED_TRANSFORMATION ( 'NONE', 'NONE', #4655,  #4154 ) ;
#688 = EDGE_CURVE ( 'NONE', #1702, #1418, #2388, .T. ) ;
#689 = B_SPLINE_CURVE_WITH_KNOTS ( 'NONE', 3,
 ( #2117, #2522, #1324, #4180, #4962, #1234, #1636, #5020 ),
 .UNSPECIFIED., .F., .F.,
 ( 4, 2, 2, 4 ),
 ( 0.007274027330054944063, 0.008608952725826013452, 0.009943878121597079373, 0.01261372891313921468 ),
 .UNSPECIFIED. ) ;
#690 = ORIENTED_EDGE ( 'NONE', *, *, #3366, .F. ) ;
#691 = EDGE_CURVE ( 'NONE', #4457, #963, #1679, .T. ) ;
#692 = PLANE ( 'NONE',  #3442 ) ;
#693 = ORIENTED_EDGE ( 'NONE', *, *, #1044, .T. ) ;
#694 = DIRECTION ( 'NONE',  ( -1.000000000000000000, 0.000000000000000000, -0.000000000000000000 ) ) ;
#695 = DIRECTION ( 'NONE',  ( -1.000000000000000000, -0.000000000000000000, -0.000000000000000000 ) ) ;
#696 = DIRECTION ( 'NONE',  ( 1.000000000000000000, 0.000000000000000000, 2.081668171172168513E-16 ) ) ;
#697 = CARTESIAN_POINT ( 'NONE',  ( -0.7500000000000000000, -9.959292143521052409, -8.787392856021027043 ) ) ;
#698 = PRESENTATION_LAYER_ASSIGNMENT (  '', '', ( #4869 ) ) ;
#699 = DIRECTION ( 'NONE',  ( 0.000000000000000000, 0.000000000000000000, 1.000000000000000000 ) ) ;
#700 = DIRECTION ( 'NONE',  ( 0.000000000000000000, 0.000000000000000000, 1.000000000000000000 ) ) ;
#701 = VERTEX_POINT ( 'NONE', #3518 ) ;
#702 = ORIENTED_EDGE ( 'NONE', *, *, #3214, .T. ) ;
#703 = CARTESIAN_POINT ( 'NONE',  ( -121.7157287525392917, 0.000000000000000000, -121.7157287525368332 ) ) ;
#704 =( NAMED_UNIT ( * ) PLANE_ANGLE_UNIT ( ) SI_UNIT ( $, .RADIAN. ) );
#705 = ORIENTED_EDGE ( 'NONE', *, *, #198, .F. ) ;
#706 = DIRECTION ( 'NONE',  ( 0.000000000000000000, -0.000000000000000000, 1.000000000000000000 ) ) ;
#707 =( NAMED_UNIT ( * ) PLANE_ANGLE_UNIT ( ) SI_UNIT ( $, .RADIAN. ) );
#708 = EDGE_CURVE ( 'NONE', #1655, #5213, #1163, .T. ) ;
#709 = EDGE_CURVE ( 'NONE', #819, #4789, #1060, .T. ) ;
#710 = EDGE_LOOP ( 'NONE', ( #1543, #1981, #3876, #3564 ) ) ;
#711 = CARTESIAN_POINT ( 'NONE',  ( -9.000000000000007105, 5.196152422706624918, -9.106320693283315393 ) ) ;
#712 = CARTESIAN_POINT ( 'NONE',  ( 0.05670911061056406466, -11.01091124578874414, -9.698321917585793983 ) ) ;
#713 = CARTESIAN_POINT ( 'NONE',  ( 9.477403599784569366, 1.836490901034003809, -9.189746347754448763 ) ) ;
#714 = DIRECTION ( 'NONE',  ( -1.000000000000000000, 0.000000000000000000, -0.000000000000000000 ) ) ;
#715 = APPLICATION_PROTOCOL_DEFINITION ( 'draft international standard', 'automotive_design', 1998, #5160 ) ;
#716 = PRODUCT_DEFINITION_SHAPE ( 'NONE', 'NONE',  #5388 ) ;
#717 = ORIENTED_EDGE ( 'NONE', *, *, #4118, .T. ) ;
#718 = EDGE_LOOP ( 'NONE', ( #2881, #2906, #4894, #4616 ) ) ;
#719 = FACE_OUTER_BOUND ( 'NONE', #24, .T. ) ;
#720 = FACE_OUTER_BOUND ( 'NONE', #3716, .T. ) ;
#721 = DIRECTION ( 'NONE',  ( 1.000000000000000000, 0.000000000000000000, 0.000000000000000000 ) ) ;
#722 = LINE ( 'NONE', #5277, #1209 ) ;
#723 = B_SPLINE_CURVE_WITH_KNOTS ( 'NONE', 3,
 ( #4029, #2769, #5306, #277, #221, #1521, #4001, #4366, #3121, #627 ),
 .UNSPECIFIED., .F., .F.,
 ( 4, 2, 2, 2, 4 ),
 ( 1.620725098399643580E-19, 0.002766603965071790135, 0.005533207930143580269, 0.008299811895215371271, 0.01106641586028715880 ),
 .UNSPECIFIED. ) ;
#724 = DIRECTION ( 'NONE',  ( 1.000000000000000000, -0.000000000000000000, -0.000000000000000000 ) ) ;
#725 = PLANE ( 'NONE',  #1977 ) ;
#726 = ORIENTED_EDGE ( 'NONE', *, *, #1041, .T. ) ;
#727 = ORIENTED_EDGE ( 'NONE', *, *, #2776, .T. ) ;
#728 = EDGE_CURVE ( 'NONE', #3383, #2814, #2200, .T. ) ;
#729 = CARTESIAN_POINT ( 'NONE',  ( 75.00000000000001421, 610.0000000000000000, 30.00000000000002487 ) ) ;
#730 = CARTESIAN_POINT ( 'NONE',  ( -25.00000000000000000, 810.0000000000000000, 24.99999999999999645 ) ) ;
#731 = CIRCLE ( 'NONE', #1938, 15.00000000000000000 ) ;
#732 = ORIENTED_EDGE ( 'NONE', *, *, #3637, .T. ) ;
#733 = CONICAL_SURFACE ( 'NONE', #1585, 5.035999999999999588, 0.7853981633974743692 ) ;
#734 = AXIS2_PLACEMENT_3D ( 'NONE', #3221, #1943, #706 ) ;
#735 = ORIENTED_EDGE ( 'NONE', *, *, #1905, .T. ) ;
#736 = CARTESIAN_POINT ( 'NONE',  ( 121.7157287525384533, 0.000000000000000000, 136.7157287525376717 ) ) ;
#737 = EDGE_CURVE ( 'NONE', #4965, #428, #3178, .T. ) ;
#738 = CYLINDRICAL_SURFACE ( 'NONE', #1107, 15.00000000000000000 ) ;
#739 = DIRECTION ( 'NONE',  ( 1.000000000000000000, -0.000000000000000000, -0.000000000000000000 ) ) ;
#740 = DIRECTION ( 'NONE',  ( 0.000000000000000000, 0.000000000000000000, 1.000000000000000000 ) ) ;
#741 = APPLICATION_PROTOCOL_DEFINITION ( 'draft international standard', 'automotive_design', 1998, #19 ) ;
#742 = EDGE_CURVE ( 'NONE', #1732, #207, #2730, .T. ) ;
#743 = ORIENTED_EDGE ( 'NONE', *, *, #4963, .F. ) ;
#744 = AXIS2_PLACEMENT_3D ( 'NONE', #3308, #4537, #1587 ) ;
#745 = VERTEX_POINT ( 'NONE', #1900 ) ;
#746 = DIRECTION ( 'NONE',  ( -0.000000000000000000, -1.000000000000000000, -0.000000000000000000 ) ) ;
#747 = DIRECTION ( 'NONE',  ( 0.000000000000000000, 0.000000000000000000, 1.000000000000000000 ) ) ;
#748 = CARTESIAN_POINT ( 'NONE',  ( 0.6000000000000033085, 0.000000000000000000, 0.000000000000000000 ) ) ;
#749 = DIRECTION ( 'NONE',  ( 1.000000000000000000, 0.000000000000000000, 0.000000000000000000 ) ) ;
#750 = CIRCLE ( 'NONE', #1517, 6.499999999999988454 ) ;
#751 = COLOUR_RGB ( '',0.8941176470588234615, 0.8941176470588234615, 0.8941176470588234615 ) ;
#752 = VERTEX_POINT ( 'NONE', #4017 ) ;
#753 = AXIS2_PLACEMENT_3D ( 'NONE', #421, #15, #1258 ) ;
#754 = VERTEX_POINT ( 'NONE', #268 ) ;
#755 =( GEOMETRIC_REPRESENTATION_CONTEXT ( 3 ) GLOBAL_UNCERTAINTY_ASSIGNED_CONTEXT ( ( #5058 ) ) GLOBAL_UNIT_ASSIGNED_CONTEXT ( ( #2393, #3976, #4011 ) ) REPRESENTATION_CONTEXT ( 'NONE', 'WORKASPACE' ) );
#756 = CARTESIAN_POINT ( 'NONE',  ( -121.7157287525392917, -20.00000000000000000, -121.7157287525368332 ) ) ;
#757 = UNCERTAINTY_MEASURE_WITH_UNIT (LENGTH_MEASURE( 1.000000000000000082E-05 ), #1560, 'distance_accuracy_value', 'NONE');
#758 = DIRECTION ( 'NONE',  ( 0.000000000000000000, 1.000000000000000000, -0.000000000000000000 ) ) ;
#759 = ORIENTED_EDGE ( 'NONE', *, *, #2279, .T. ) ;
#760 = ADVANCED_FACE ( 'NONE', ( #5235 ), #3158, .T. ) ;
#761 = VECTOR ( 'NONE', #2328, 1000.000000000000000 ) ;
#762 = EDGE_CURVE ( 'NONE', #1094, #3611, #3337, .T. ) ;
#763 = AXIS2_PLACEMENT_3D ( 'NONE', #3258, #1554, #4883 ) ;
#764 = ORIENTED_EDGE ( 'NONE', *, *, #1472, .T. ) ;
#765 = ORIENTED_EDGE ( 'NONE', *, *, #433, .F. ) ;
#766 = DIRECTION ( 'NONE',  ( 0.000000000000000000, 0.000000000000000000, 1.000000000000000000 ) ) ;
#767 = ORIENTED_EDGE ( 'NONE', *, *, #3722, .F. ) ;
#768 =( GEOMETRIC_REPRESENTATION_CONTEXT ( 3 ) GLOBAL_UNCERTAINTY_ASSIGNED_CONTEXT ( ( #2886 ) ) GLOBAL_UNIT_ASSIGNED_CONTEXT ( ( #2204, #5209, #5150 ) ) REPRESENTATION_CONTEXT ( 'NONE', 'WORKASPACE' ) );
#769 = DIRECTION ( 'NONE',  ( 1.000000000000000000, 0.000000000000000000, 0.000000000000000000 ) ) ;
#770 = ORIENTED_EDGE ( 'NONE', *, *, #2624, .F. ) ;
#771 = VECTOR ( 'NONE', #4476, 1000.000000000000000 ) ;
#772 = EDGE_LOOP ( 'NONE', ( #4541, #1846 ) ) ;
#773 = CARTESIAN_POINT ( 'NONE',  ( 165.0000000000000000, 870.0000000000000000, 6.000000000000001776 ) ) ;
#774 = CYLINDRICAL_SURFACE ( 'NONE', #4248, 5.999999999999998224 ) ;
#775 = DIRECTION ( 'NONE',  ( 0.000000000000000000, -1.000000000000000000, 0.000000000000000000 ) ) ;
#776 = DIRECTION ( 'NONE',  ( 1.000000000000000000, 0.000000000000000000, 0.000000000000000000 ) ) ;
#777 = VECTOR ( 'NONE', #442, 1000.000000000000000 ) ;
#778 = ITEM_DEFINED_TRANSFORMATION ( 'NONE', 'NONE', #3020,  #4154 ) ;
#779 = ADVANCED_FACE ( 'NONE', ( #1231 ), #2935, .T. ) ;
#780 = AXIS2_PLACEMENT_3D ( 'NONE', #945, #4750, #2176 ) ;
#781 = DIRECTION ( 'NONE',  ( 0.000000000000000000, -0.000000000000000000, 1.000000000000000000 ) ) ;
#782 = ORIENTED_EDGE ( 'NONE', *, *, #5242, .T. ) ;
#783 = CARTESIAN_POINT ( 'NONE',  ( 0.000000000000000000, -10.39230484541327293, -8.935996291721338025 ) ) ;
#784 = DIRECTION ( 'NONE',  ( -1.000000000000000000, -0.000000000000000000, -0.000000000000000000 ) ) ;
#785 = CARTESIAN_POINT ( 'NONE',  ( 6.000000000000000000, 0.000000000000000000, 0.000000000000000000 ) ) ;
#786 = CARTESIAN_POINT ( 'NONE',  ( 139.9999999999999716, 885.0000000000000000, -25.00000000000000000 ) ) ;
#787 = EDGE_CURVE ( 'NONE', #1913, #3047, #981, .T. ) ;
#788 = APPLICATION_CONTEXT ( 'automotive_design' ) ;
#789 = DIRECTION ( 'NONE',  ( 0.5000000000000004441, -0.8660254037844384856, 0.000000000000000000 ) ) ;
#790 = CARTESIAN_POINT ( 'NONE',  ( -0.7500000000000007772, 9.959292143521045304, -8.787392856021023491 ) ) ;
#791 = VERTEX_POINT ( 'NONE', #4572 ) ;
#792 = ORIENTED_EDGE ( 'NONE', *, *, #2169, .F. ) ;
#793 = FACE_OUTER_BOUND ( 'NONE', #4731, .T. ) ;
#794 = EDGE_CURVE ( 'NONE', #4433, #2174, #1143, .T. ) ;
#795 = ORIENTED_EDGE ( 'NONE', *, *, #3460, .F. ) ;
#796 = ORIENTED_EDGE ( 'NONE', *, *, #4341, .F. ) ;
#797 = CARTESIAN_POINT ( 'NONE',  ( 25.00000000000000000, 610.0000000000000000, 25.00000000000000711 ) ) ;
#798 = CARTESIAN_POINT ( 'NONE',  ( -1.499235438992549296, 10.09238013696277037, -9.361164777501199907 ) ) ;
#799 = DIRECTION ( 'NONE',  ( -1.000000000000000000, 0.000000000000000000, -9.251858538542972814E-17 ) ) ;
#800 = LINE ( 'NONE', #247, #2779 ) ;
#801 = APPLICATION_PROTOCOL_DEFINITION ( 'draft international standard', 'automotive_design', 1998, #4842 ) ;
#802 = ADVANCED_FACE ( 'NONE', ( #1172 ), #38, .F. ) ;
#803 = CIRCLE ( 'NONE', #1475, 6.499999999999988454 ) ;
#804 = DIRECTION ( 'NONE',  ( 0.000000000000000000, -0.000000000000000000, -1.000000000000000000 ) ) ;
#805 = ORIENTED_EDGE ( 'NONE', *, *, #4792, .T. ) ;
#806 = CARTESIAN_POINT ( 'NONE',  ( 0.000000000000000000, 839.0360000000000582, 0.000000000000000000 ) ) ;
#807 = COLOUR_RGB ( '',0.8941176470588234615, 0.8941176470588234615, 0.8941176470588234615 ) ;
#808 = DIRECTION ( 'NONE',  ( 0.000000000000000000, 0.000000000000000000, -1.000000000000000000 ) ) ;
#809 = CARTESIAN_POINT ( 'NONE',  ( 137.5000000000000000, 870.0000000000000000, 0.000000000000000000 ) ) ;
#810 = ORIENTED_EDGE ( 'NONE', *, *, #233, .F. ) ;
#811 = LINE ( 'NONE', #4169, #51 ) ;
#812 = CARTESIAN_POINT ( 'NONE',  ( -1.144917494144692998E-14, 570.0000000000000000, 30.00000000000001066 ) ) ;
#813 = VERTEX_POINT ( 'NONE', #2815 ) ;
#814 = EDGE_CURVE ( 'NONE', #3015, #3385, #852, .T. ) ;
#815 = ORIENTED_EDGE ( 'NONE', *, *, #4633, .T. ) ;
#816 = ORIENTED_EDGE ( 'NONE', *, *, #5242, .F. ) ;
#817 = EDGE_CURVE ( 'NONE', #4457, #4555, #3001, .T. ) ;
#818 = CYLINDRICAL_SURFACE ( 'NONE', #2939, 5.099999999999999645 ) ;
#819 = VERTEX_POINT ( 'NONE', #797 ) ;
#820 = ORIENTED_EDGE ( 'NONE', *, *, #3637, .F. ) ;
#821 = DIRECTION ( 'NONE',  ( -0.000000000000000000, 1.000000000000000000, 1.224646799147353207E-16 ) ) ;
#822 = CARTESIAN_POINT ( 'NONE',  ( -8.758033615148283602, 5.911365213026127385, -9.525564194215435876 ) ) ;
#823 = DIRECTION ( 'NONE',  ( -1.000000000000000000, 0.000000000000000000, 0.000000000000000000 ) ) ;
#824 = CARTESIAN_POINT ( 'NONE',  ( 7.950863337915118123, -6.367515845290791177, -9.383905213721023486 ) ) ;
#825 = VECTOR ( 'NONE', #3989, 999.9999999999998863 ) ;
#826 = AXIS2_PLACEMENT_3D ( 'NONE', #3603, #1034, #1920 ) ;
#827 = ORIENTED_EDGE ( 'NONE', *, *, #5184, .F. ) ;
#828 = FACE_OUTER_BOUND ( 'NONE', #1816, .T. ) ;
#829 = EDGE_CURVE ( 'NONE', #3578, #1196, #3313, .T. ) ;
#830 = LINE ( 'NONE', #3422, #4489 ) ;
#831 = DIRECTION ( 'NONE',  ( -1.000000000000000000, 0.000000000000000000, 0.000000000000000000 ) ) ;
#832 = CIRCLE ( 'NONE', #2303, 9.000000000000001776 ) ;
#833 = EDGE_LOOP ( 'NONE', ( #796, #4382, #5344, #886, #4460 ) ) ;
#834 = LINE ( 'NONE', #4115, #1093 ) ;
#835 = DIRECTION ( 'NONE',  ( 0.000000000000000000, -0.4999999999999989453, 0.8660254037844392627 ) ) ;
#836 = CIRCLE ( 'NONE', #1178, 6.000000000000005329 ) ;
#837 = ORIENTED_EDGE ( 'NONE', *, *, #4975, .T. ) ;
#838 = VERTEX_POINT ( 'NONE', #4461 ) ;
#839 = AXIS2_PLACEMENT_3D ( 'NONE', #349, #4430, #864 ) ;
#840 = PRODUCT_DEFINITION_FORMATION_WITH_SPECIFIED_SOURCE ( 'ANY', '', #918, .NOT_KNOWN. ) ;
#841 = AXIS2_PLACEMENT_3D ( 'NONE', #5311, #2025, #2001 ) ;
#842 = EDGE_CURVE ( 'NONE', #3267, #4388, #3750, .T. ) ;
#843 = CYLINDRICAL_SURFACE ( 'NONE', #2403, 6.500000000000000000 ) ;
#844 = ORIENTED_EDGE ( 'NONE', *, *, #814, .F. ) ;
#845 = FILL_AREA_STYLE ('',( #3720 ) ) ;
#846 = ORIENTED_EDGE ( 'NONE', *, *, #2312, .F. ) ;
#847 = AXIS2_PLACEMENT_3D ( 'NONE', #2606, #3446, #2183 ) ;
#848 = ADVANCED_FACE ( 'NONE', ( #4987 ), #410, .T. ) ;
#849 = VECTOR ( 'NONE', #191, 1000.000000000000000 ) ;
#850 = VERTEX_POINT ( 'NONE', #5295 ) ;
#851 = EDGE_LOOP ( 'NONE', ( #978, #1701, #2976, #2915 ) ) ;
#852 = LINE ( 'NONE', #2846, #116 ) ;
#853 = CARTESIAN_POINT ( 'NONE',  ( -2.790577774332636096, 8.781164016207728906, -8.465119797812908686 ) ) ;
#854 = DIRECTION ( 'NONE',  ( 0.000000000000000000, 0.000000000000000000, -1.000000000000000000 ) ) ;
#855 = CYLINDRICAL_SURFACE ( 'NONE', #1148, 5.999999999999998224 ) ;
#856 = DIRECTION ( 'NONE',  ( -1.000000000000000000, 0.000000000000000000, 0.000000000000000000 ) ) ;
#857 = VECTOR ( 'NONE', #2717, 1000.000000000000000 ) ;
#858 = CARTESIAN_POINT ( 'NONE',  ( 0.000000000000000000, 570.0000000000000000, 30.00000000000000711 ) ) ;
#859 = EDGE_CURVE ( 'NONE', #1603, #207, #1544, .T. ) ;
#860 = CARTESIAN_POINT ( 'NONE',  ( -9.507358266631047883, 5.552911536195821895, -9.698012930120947672 ) ) ;
#861 = VECTOR ( 'NONE', #3140, 1000.000000000000000 ) ;
#862 = EDGE_CURVE ( 'NONE', #4388, #5233, #1567, .T. ) ;
#863 = ORIENTED_EDGE ( 'NONE', *, *, #517, .T. ) ;
#864 = DIRECTION ( 'NONE',  ( 1.000000000000000000, 0.000000000000000000, 0.000000000000000000 ) ) ;
#865 = CARTESIAN_POINT ( 'NONE',  ( 2.893723230124677137, 8.721612959541547028, -9.019248292997474437 ) ) ;
#866 = FACE_OUTER_BOUND ( 'NONE', #2540, .T. ) ;
#867 = ORIENTED_EDGE ( 'NONE', *, *, #4375, .F. ) ;
#868 = FACE_OUTER_BOUND ( 'NONE', #5245, .T. ) ;
#869 = EDGE_LOOP ( 'NONE', ( #1482, #1899, #1551, #4613 ) ) ;
#870 = VERTEX_POINT ( 'NONE', #736 ) ;
#871 = VERTEX_POINT ( 'NONE', #2071 ) ;
#872 = FACE_OUTER_BOUND ( 'NONE', #66, .T. ) ;
#873 = FACE_BOUND ( 'NONE', #4726, .T. ) ;
#874 = CYLINDRICAL_SURFACE ( 'NONE', #4672, 6.000000000000006217 ) ;
#875 = ADVANCED_FACE ( 'NONE', ( #4126 ), #1205, .T. ) ;
#876 = EDGE_CURVE ( 'NONE', #3385, #3280, #4904, .T. ) ;
#877 = FACE_OUTER_BOUND ( 'NONE', #4794, .T. ) ;
#878 = ORIENTED_EDGE ( 'NONE', *, *, #3994, .T. ) ;
#879 = CARTESIAN_POINT ( 'NONE',  ( -150.0000000000000000, 810.0000000000000000, 25.00000000000000000 ) ) ;
#880 = CARTESIAN_POINT ( 'NONE',  ( 0.000000000000000000, 0.000000000000000000, -10.20000000000000107 ) ) ;
#881 = CARTESIAN_POINT ( 'NONE',  ( 25.00000000000000000, 210.0000000000000284, -25.00000000000000000 ) ) ;
#882 = DIRECTION ( 'NONE',  ( 0.000000000000000000, -1.039664082171044284E-15, -1.000000000000000000 ) ) ;
#883 = ORIENTED_EDGE ( 'NONE', *, *, #876, .F. ) ;
#884 = CARTESIAN_POINT ( 'NONE',  ( 5.999999999999983125, 570.0000000000000000, -24.03599999999999071 ) ) ;
#885 = CARTESIAN_POINT ( 'NONE',  ( 9.000000000000001776, 4.367518130255698239, -0.8586158810094328686 ) ) ;
#886 = ORIENTED_EDGE ( 'NONE', *, *, #1154, .T. ) ;
#887 = CARTESIAN_POINT ( 'NONE',  ( 7.552115898706448505, -6.032088698343846644, -0.5428950306860315100 ) ) ;
#888 = ORIENTED_EDGE ( 'NONE', *, *, #961, .T. ) ;
#889 = CARTESIAN_POINT ( 'NONE',  ( 0.000000000000000000, 60.00000000000000711, 0.000000000000000000 ) ) ;
#890 = CARTESIAN_POINT ( 'NONE',  ( -1.676835913137321903E-15, 35.00000000000000000, -30.00000000000000711 ) ) ;
#891 = DIRECTION ( 'NONE',  ( 0.000000000000000000, 0.000000000000000000, -1.000000000000000000 ) ) ;
#892 = CARTESIAN_POINT ( 'NONE',  ( 5.303004762135293149, -7.330613618480590787, -8.460795847314498630 ) ) ;
#893 = B_SPLINE_CURVE_WITH_KNOTS ( 'NONE', 3,
 ( #3621, #3684, #1159, #1269, #1583, #1133, #2801, #3661, #3266 ),
 .UNSPECIFIED., .F., .F.,
 ( 4, 2, 1, 2, 4 ),
 ( 0.000000000000000000, 0.002598076211353316303, 0.005196152422706632606, 0.007794228634059949777, 0.01039230484541326521 ),
 .UNSPECIFIED. ) ;
#894 = EDGE_CURVE ( 'NONE', #1603, #3270, #4807, .T. ) ;
#895 = CARTESIAN_POINT ( 'NONE',  ( -5.010000000000002451, 6.135480463728242006E-16, -0.6932054628276118624 ) ) ;
#896 = DIRECTION ( 'NONE',  ( -0.7071067811865577868, 0.000000000000000000, 0.7071067811865373587 ) ) ;
#897 = SURFACE_STYLE_FILL_AREA ( #4967 ) ;
#898 = CARTESIAN_POINT ( 'NONE',  ( 5.099999999999999645, 0.000000000000000000, -11.34441321561125626 ) ) ;
#899 = CARTESIAN_POINT ( 'NONE',  ( -9.000000000000000000, -5.678788000576118655, -9.021742658504674495 ) ) ;
#900 = VECTOR ( 'NONE', #3282, 1000.000000000000000 ) ;
#901 = VECTOR ( 'NONE', #2965, 1000.000000000000000 ) ;
#902 = ORIENTED_EDGE ( 'NONE', *, *, #98, .F. ) ;
#903 = ORIENTED_EDGE ( 'NONE', *, *, #2485, .F. ) ;
#904 = DIRECTION ( 'NONE',  ( 0.000000000000000000, 0.000000000000000000, -1.000000000000000000 ) ) ;
#905 = CARTESIAN_POINT ( 'NONE',  ( 9.000000000000000000, 5.196152422706636465, -1.199999999999999734 ) ) ;
#906 = VECTOR ( 'NONE', #371, 1000.000000000000000 ) ;
#907 = CARTESIAN_POINT ( 'NONE',  ( -1.144917494144692998E-14, 570.0000000000000000, 30.00000000000001066 ) ) ;
#908 = EDGE_CURVE ( 'NONE', #4532, #4353, #4554, .T. ) ;
#909 = AXIS2_PLACEMENT_3D ( 'NONE', #907, #510, #3839 ) ;
#910 = STYLED_ITEM ( 'NONE', ( #4984 ), #119 ) ;
#911 = ADVANCED_FACE ( 'NONE', ( #2175 ), #2619, .T. ) ;
#912 = ORIENTED_EDGE ( 'NONE', *, *, #533, .F. ) ;
#913 = AXIS2_PLACEMENT_3D ( 'NONE', #2357, #2823, #808 ) ;
#914 = FACE_BOUND ( 'NONE', #4721, .T. ) ;
#915 = CARTESIAN_POINT ( 'NONE',  ( 2.999999999999998668, 8.660254037844387298, -8.505011083697294083 ) ) ;
#916 =( GEOMETRIC_REPRESENTATION_CONTEXT ( 3 ) GLOBAL_UNCERTAINTY_ASSIGNED_CONTEXT ( ( #2996 ) ) GLOBAL_UNIT_ASSIGNED_CONTEXT ( ( #5130, #4728, #624 ) ) REPRESENTATION_CONTEXT ( 'NONE', 'WORKASPACE' ) );
#917 = PLANE ( 'NONE',  #130 ) ;
#918 = PRODUCT ( 'Outer Column Guide Sleeve', 'Outer Column Guide Sleeve', '', ( #3228 ) ) ;
#919 = ITEM_DEFINED_TRANSFORMATION ( 'NONE', 'NONE', #3731,  #4154 ) ;
#920 = AXIS2_PLACEMENT_3D ( 'NONE', #2464, #4463, #2817 ) ;
#921 = CIRCLE ( 'NONE', #2511, 5.999999999999894307 ) ;
#922 = CARTESIAN_POINT ( 'NONE',  ( -8.999999999999998224, 3.519160108721328228, -0.5651793076691160600 ) ) ;
#923 = CARTESIAN_POINT ( 'NONE',  ( 9.477420239195661011, -1.840077440320891045, -9.189982433786857641 ) ) ;
#924 = DIRECTION ( 'NONE',  ( 1.000000000000000000, 0.000000000000000000, 0.000000000000000000 ) ) ;
#925 = ORIENTED_EDGE ( 'NONE', *, *, #5286, .F. ) ;
#926 = DIRECTION ( 'NONE',  ( 1.000000000000000000, 0.000000000000000000, -0.000000000000000000 ) ) ;
#927 = ORIENTED_EDGE ( 'NONE', *, *, #4973, .F. ) ;
#928 = VECTOR ( 'NONE', #4600, 1000.000000000000000 ) ;
#929 =( NAMED_UNIT ( * ) SI_UNIT ( $, .STERADIAN. ) SOLID_ANGLE_UNIT ( ) );
#930 = ADVANCED_FACE ( 'NONE', ( #914, #5090, #872, #3823, #2115, #1280 ), #5121, .F. ) ;
#931 = CIRCLE ( 'NONE', #3993, 6.499999999999988454 ) ;
#932 = VERTEX_POINT ( 'NONE', #3393 ) ;
#933 =( NAMED_UNIT ( * ) SI_UNIT ( $, .STERADIAN. ) SOLID_ANGLE_UNIT ( ) );
#934 = DIRECTION ( 'NONE',  ( -1.000000000000000000, 0.000000000000000000, 0.000000000000000000 ) ) ;
#935 = FACE_BOUND ( 'NONE', #291, .T. ) ;
#936 = VECTOR ( 'NONE', #623, 1000.000000000000000 ) ;
#937 = EDGE_CURVE ( 'NONE', #4400, #601, #5166, .T. ) ;
#938 = EDGE_CURVE ( 'NONE', #3516, #2213, #468, .T. ) ;
#939 = DIRECTION ( 'NONE',  ( -0.000000000000000000, -0.000000000000000000, 1.000000000000000000 ) ) ;
#940 = EDGE_CURVE ( 'NONE', #1913, #5142, #3077, .T. ) ;
#941 = ORIENTED_EDGE ( 'NONE', *, *, #1301, .T. ) ;
#942 =( NAMED_UNIT ( * ) SI_UNIT ( $, .STERADIAN. ) SOLID_ANGLE_UNIT ( ) );
#943 =( REPRESENTATION_RELATIONSHIP ('NONE','NONE', #4791, #3275 ) REPRESENTATION_RELATIONSHIP_WITH_TRANSFORMATION ( #2017 )SHAPE_REPRESENTATION_RELATIONSHIP( ) );
#944 = DIRECTION ( 'NONE',  ( -1.000000000000000000, 0.000000000000000000, -2.081668171172168513E-16 ) ) ;
#945 = CARTESIAN_POINT ( 'NONE',  ( 0.000000000000000000, 510.0000000000000000, 25.00000000000000000 ) ) ;
#946 = CARTESIAN_POINT ( 'NONE',  ( -9.000000000000001776, 0.000000000000000000, 0.000000000000000000 ) ) ;
#947 = DIRECTION ( 'NONE',  ( -1.000000000000000000, 0.000000000000000000, 0.000000000000000000 ) ) ;
#948 = DIRECTION ( 'NONE',  ( -1.000000000000000000, -0.000000000000000000, -0.000000000000000000 ) ) ;
#949 = DIRECTION ( 'NONE',  ( -1.000000000000000000, 0.000000000000000000, 0.000000000000000000 ) ) ;
#950 = DIRECTION ( 'NONE',  ( -1.000000000000000000, -0.000000000000000000, 0.000000000000000000 ) ) ;
#951 = FILL_AREA_STYLE_COLOUR ( '', #1708 ) ;
#952 = ADVANCED_FACE ( 'NONE', ( #3437 ), #2207, .T. ) ;
#953 = CARTESIAN_POINT ( 'NONE',  ( 75.00000000000001421, 610.0000000000000000, 50.00000000000002132 ) ) ;
#954 = ORIENTED_EDGE ( 'NONE', *, *, #3467, .T. ) ;
#955 = DIRECTION ( 'NONE',  ( 0.000000000000000000, -1.000000000000000000, 0.000000000000000000 ) ) ;
#956 = CARTESIAN_POINT ( 'NONE',  ( -24.99999999999999645, 210.0000000000000284, -25.00000000000000000 ) ) ;
#957 = CARTESIAN_POINT ( 'NONE',  ( 9.000000000000000000, 5.196152422706636465, -1.199999999999999734 ) ) ;
#958 = UNCERTAINTY_MEASURE_WITH_UNIT (LENGTH_MEASURE( 1.000000000000000082E-05 ), #2410, 'distance_accuracy_value', 'NONE');
#959 = DIRECTION ( 'NONE',  ( -0.000000000000000000, -0.000000000000000000, 1.000000000000000000 ) ) ;
#960 = DIRECTION ( 'NONE',  ( 0.000000000000000000, -1.000000000000000000, 1.039664082171044284E-15 ) ) ;
#961 = EDGE_CURVE ( 'NONE', #4929, #3556, #3052, .T. ) ;
#962 = VECTOR ( 'NONE', #3089, 1000.000000000000000 ) ;
#963 = VERTEX_POINT ( 'NONE', #2198 ) ;
#964 = ADVANCED_FACE ( 'NONE', ( #2979 ), #1321, .T. ) ;
#965 = VECTOR ( 'NONE', #2398, 1000.000000000000000 ) ;
#966 = VERTEX_POINT ( 'NONE', #3415 ) ;
#967 = CARTESIAN_POINT ( 'NONE',  ( -9.477420239195661011, 1.840077440320891711, -9.189982433786857641 ) ) ;
#968 = DIRECTION ( 'NONE',  ( -1.000000000000000000, -0.000000000000000000, -0.000000000000000000 ) ) ;
#969 = CARTESIAN_POINT ( 'NONE',  ( 25.00000000000000000, 610.0000000000000000, 25.00000000000000711 ) ) ;
#970 = DIRECTION ( 'NONE',  ( -0.000000000000000000, -0.000000000000000000, 1.000000000000000000 ) ) ;
#971 = CARTESIAN_POINT ( 'NONE',  ( 0.000000000000000000, 570.0000000000000000, -25.00000000000000000 ) ) ;
#972 = DIRECTION ( 'NONE',  ( -1.000000000000000000, -0.000000000000000000, -2.775557561562891351E-16 ) ) ;
#973 = CARTESIAN_POINT ( 'NONE',  ( 9.000000000000000000, -5.196152422706636465, -12.00000000000000000 ) ) ;
#974 = ORIENTED_EDGE ( 'NONE', *, *, #39, .F. ) ;
#975 = DIRECTION ( 'NONE',  ( 1.000000000000000000, 0.000000000000000000, 0.000000000000000000 ) ) ;
#976 = PRODUCT ( 'hex flange nut gradea_iso_ISO - 4161 - M12 - N', 'hex flange nut gradea_iso_ISO - 4161 - M12 - N', '', ( #5267 ) ) ;
#977 = CARTESIAN_POINT ( 'NONE',  ( 0.000000000000000000, 0.000000000000000000, 0.000000000000000000 ) ) ;
#978 = ORIENTED_EDGE ( 'NONE', *, *, #1193, .T. ) ;
#979 = PRODUCT_DEFINITION ( 'UNKNOWN', '', #565, #1182 ) ;
#980 = CARTESIAN_POINT ( 'NONE',  ( 9.000000000000003553, -1.784038208492157551, -0.1183376658062880588 ) ) ;
#981 = CIRCLE ( 'NONE', #552, 0.5999999999999998668 ) ;
#982 = ORIENTED_EDGE ( 'NONE', *, *, #1792, .F. ) ;
#983 = CARTESIAN_POINT ( 'NONE',  ( 6.000000000000000000, 5.839897972853065333, -6.938893903907228378E-15 ) ) ;
#984 = LINE ( 'NONE', #1407, #145 ) ;
#985 = CARTESIAN_POINT ( 'NONE',  ( 0.000000000000000000, 810.0000000000000000, 0.000000000000000000 ) ) ;
#986 = DIRECTION ( 'NONE',  ( -0.000000000000000000, -0.000000000000000000, 1.000000000000000000 ) ) ;
#987 = TOROIDAL_SURFACE ( 'NONE', #2035, 6.600000000000001421, 0.5999999999999999778 ) ;
#988 = CARTESIAN_POINT ( 'NONE',  ( 0.000000000000000000, 570.0000000000000000, 25.00000000000000000 ) ) ;
#989 = VECTOR ( 'NONE', #1784, 1000.000000000000000 ) ;
#990 = FILL_AREA_STYLE_COLOUR ( '', #653 ) ;
#991 = ORIENTED_EDGE ( 'NONE', *, *, #4856, .T. ) ;
#992 = EDGE_CURVE ( 'NONE', #1518, #3842, #1759, .T. ) ;
#993 = ORIENTED_EDGE ( 'NONE', *, *, #3708, .T. ) ;
#994 = DIRECTION ( 'NONE',  ( 0.000000000000000000, 0.8660254037844381525, -0.5000000000000008882 ) ) ;
#995 = DIRECTION ( 'NONE',  ( -0.000000000000000000, -1.000000000000000000, -0.000000000000000000 ) ) ;
#996 = CARTESIAN_POINT ( 'NONE',  ( 165.0000000000000000, 870.0000000000000000, -5.036000000000040444 ) ) ;
#997 = AXIS2_PLACEMENT_3D ( 'NONE', #201, #1860, #5201 ) ;
#998 = AXIS2_PLACEMENT_3D ( 'NONE', #1508, #1083, #4072 ) ;
#999 = VECTOR ( 'NONE', #3243, 1000.000000000000000 ) ;
#1000 = PRESENTATION_LAYER_ASSIGNMENT (  '', '', ( #491 ) ) ;
#1001 = ORIENTED_EDGE ( 'NONE', *, *, #1491, .F. ) ;
#1002 = ORIENTED_EDGE ( 'NONE', *, *, #3242, .T. ) ;
#1003 = EDGE_LOOP ( 'NONE', ( #4168, #2495 ) ) ;
#1004 = DIRECTION ( 'NONE',  ( -1.000000000000000000, -0.000000000000000000, -0.000000000000000000 ) ) ;
#1005 = DIRECTION ( 'NONE',  ( 0.000000000000000000, -0.000000000000000000, 1.000000000000000000 ) ) ;
#1006 = CARTESIAN_POINT ( 'NONE',  ( 121.7157287525372311, -20.00000000000000000, -121.7157287525388369 ) ) ;
#1007 = ORIENTED_EDGE ( 'NONE', *, *, #2705, .F. ) ;
#1008 = PLANE ( 'NONE',  #1116 ) ;
#1009 = CARTESIAN_POINT ( 'NONE',  ( 0.000000000000000000, 0.000000000000000000, 0.000000000000000000 ) ) ;
#1010 = VECTOR ( 'NONE', #1523, 999.9999999999998863 ) ;
#1011 = AXIS2_PLACEMENT_3D ( 'NONE', #2490, #2911, #4155 ) ;
#1012 = PRODUCT_DEFINITION_SHAPE ( 'NONE', 'NONE',  #5387 ) ;
#1013 = EDGE_LOOP ( 'NONE', ( #4222, #3217 ) ) ;
#1014 = ADVANCED_FACE ( 'NONE', ( #3469 ), #5085, .T. ) ;
#1015 = CARTESIAN_POINT ( 'NONE',  ( -1.144917494144692998E-14, 570.0000000000000000, -24.03599999999999071 ) ) ;
#1016 = DIRECTION ( 'NONE',  ( 0.000000000000000000, 0.000000000000000000, -1.000000000000000000 ) ) ;
#1017 = LINE ( 'NONE', #4706, #2766 ) ;
#1018 = AXIS2_PLACEMENT_3D ( 'NONE', #2079, #4161, #2987 ) ;
#1019 = DIRECTION ( 'NONE',  ( -0.000000000000000000, -0.000000000000000000, -1.000000000000000000 ) ) ;
#1020 = FACE_OUTER_BOUND ( 'NONE', #1227, .T. ) ;
#1021 = EDGE_CURVE ( 'NONE', #1591, #4832, #555, .T. ) ;
#1022 = AXIS2_PLACEMENT_3D ( 'NONE', #2060, #3741, #3211 ) ;
#1023 =( REPRESENTATION_RELATIONSHIP ('NONE','NONE', #4791, #302 ) REPRESENTATION_RELATIONSHIP_WITH_TRANSFORMATION ( #414 )SHAPE_REPRESENTATION_RELATIONSHIP( ) );
#1024 = LINE ( 'NONE', #1388, #1958 ) ;
#1025 = CARTESIAN_POINT ( 'NONE',  ( -121.7157287525381122, -20.00000000000000000, 121.7157287525380127 ) ) ;
#1026 = VECTOR ( 'NONE', #700, 1000.000000000000000 ) ;
#1027 = ORIENTED_EDGE ( 'NONE', *, *, #2170, .F. ) ;
#1028 =( NAMED_UNIT ( * ) PLANE_ANGLE_UNIT ( ) SI_UNIT ( $, .RADIAN. ) );
#1029 = EDGE_CURVE ( 'NONE', #2213, #3516, #1411, .T. ) ;
#1030 = AXIS2_PLACEMENT_3D ( 'NONE', #4574, #3774, #413 ) ;
#1031 = ORIENTED_EDGE ( 'NONE', *, *, #507, .F. ) ;
#1032 = DIRECTION ( 'NONE',  ( -0.000000000000000000, 1.000000000000000000, -0.000000000000000000 ) ) ;
#1033 = ORIENTED_EDGE ( 'NONE', *, *, #1852, .T. ) ;
#1034 = DIRECTION ( 'NONE',  ( 0.000000000000000000, -1.000000000000000000, 0.000000000000000000 ) ) ;
#1035 = CARTESIAN_POINT ( 'NONE',  ( -121.7157287525392917, -20.00000000000000000, -106.7157287525368332 ) ) ;
#1036 = ORIENTED_EDGE ( 'NONE', *, *, #3071, .T. ) ;
#1037 = ORIENTED_EDGE ( 'NONE', *, *, #2742, .F. ) ;
#1038 = DIRECTION ( 'NONE',  ( 0.000000000000000000, 0.000000000000000000, -1.000000000000000000 ) ) ;
#1039 = SURFACE_SIDE_STYLE ('',( #2708 ) ) ;
#1040 = PLANE ( 'NONE',  #3295 ) ;
#1041 = EDGE_CURVE ( 'NONE', #3303, #457, #1786, .T. ) ;
#1042 = LINE ( 'NONE', #2710, #936 ) ;
#1043 = DIRECTION ( 'NONE',  ( -1.000000000000000000, 0.000000000000000000, 0.000000000000000000 ) ) ;
#1044 = EDGE_CURVE ( 'NONE', #3246, #871, #5265, .T. ) ;
#1045 = EDGE_LOOP ( 'NONE', ( #5269, #1939, #430, #4843 ) ) ;
#1046 = CARTESIAN_POINT ( 'NONE',  ( 2.951638237467836046, -8.688175714460822263, -0.1192015822679215187 ) ) ;
#1047 = CARTESIAN_POINT ( 'NONE',  ( 0.000000000000000000, -2.919948986426526893, 5.057500000000001883 ) ) ;
#1048 = LINE ( 'NONE', #4368, #1525 ) ;
#1049 = CARTESIAN_POINT ( 'NONE',  ( -30.00000000000000355, 610.0000000000000000, 30.00000000000000000 ) ) ;
#1050 = CARTESIAN_POINT ( 'NONE',  ( 9.000000000000000000, 3.792226493019370093, -8.707316330048348263 ) ) ;
#1051 = CARTESIAN_POINT ( 'NONE',  ( -24.99999999999999645, 810.0000000000000000, -25.00000000000000000 ) ) ;
#1052 = ORIENTED_EDGE ( 'NONE', *, *, #4879, .T. ) ;
#1053 = VECTOR ( 'NONE', #5134, 1000.000000000000000 ) ;
#1054 = ORIENTED_EDGE ( 'NONE', *, *, #4694, .T. ) ;
#1055 = DIRECTION ( 'NONE',  ( -1.000000000000000000, 0.000000000000000000, 0.000000000000000000 ) ) ;
#1056 = CARTESIAN_POINT ( 'NONE',  ( 6.000000000000000000, -2.919948986426526893, 5.057500000000001883 ) ) ;
#1057 = PLANE ( 'NONE',  #5183 ) ;
#1058 = ORIENTED_EDGE ( 'NONE', *, *, #1878, .F. ) ;
#1059 = ORIENTED_EDGE ( 'NONE', *, *, #1669, .T. ) ;
#1060 = LINE ( 'NONE', #4411, #5259 ) ;
#1061 = LINE ( 'NONE', #2731, #2423 ) ;
#1062 = FACE_BOUND ( 'NONE', #2196, .T. ) ;
#1063 = LINE ( 'NONE', #3084, #861 ) ;
#1064 = DIRECTION ( 'NONE',  ( 6.123233995736766036E-17, 0.000000000000000000, -1.000000000000000000 ) ) ;
#1065 = SHAPE_REPRESENTATION ( 'Outer Column Guide Sleeve', ( #4154 ), #3189 ) ;
#1066 = EDGE_CURVE ( 'NONE', #2454, #4719, #118, .T. ) ;
#1067 = CARTESIAN_POINT ( 'NONE',  ( -121.7157287525381122, -20.00000000000000000, 106.7157287525380127 ) ) ;
#1068 = LINE ( 'NONE', #2631, #4741 ) ;
#1069 = CARTESIAN_POINT ( 'NONE',  ( 30.00000000000000355, 610.0000000000000000, 0.000000000000000000 ) ) ;
#1070 = FACE_OUTER_BOUND ( 'NONE', #3392, .T. ) ;
#1071 = CIRCLE ( 'NONE', #4136, 6.000000000000000888 ) ;
#1072 =( BOUNDED_SURFACE ( )  B_SPLINE_SURFACE ( 3, 2, ( 
 ( #2463, #2544, #1714 ),
 ( #4520, #2569, #798 ),
 ( #853, #2072, #1633 ),
 ( #56, #490, #1597 ),
 ( #460, #5045, #4127 ),
 ( #3727, #3773, #3752 ),
 ( #3283, #3338, #822 ),
 ( #4988, #5348, #2149 ) ),
 .UNSPECIFIED., .F., .F., .T. ) 
 B_SPLINE_SURFACE_WITH_KNOTS ( ( 4, 2, 2, 4 ),
 ( 3, 3 ),
 ( 0.04613854442509285336, 0.05169925677048779755, 0.05447961294318526965, 0.05725996911588274174 ),
 ( 0.000000000000000000, 1.000000000000000000 ),
 .UNSPECIFIED. ) 
 GEOMETRIC_REPRESENTATION_ITEM ( )  RATIONAL_B_SPLINE_SURFACE ( (
 ( 1.000000000000000000, 0.8047781684971931915, 1.000000000000000000),
 ( 1.000000000000000000, 0.8123765127742886838, 1.000000000000000000),
 ( 1.000000000000000000, 0.8190661184400637174, 1.000000000000000000),
 ( 1.000000000000000000, 0.8191936944252291575, 1.000000000000000000),
 ( 1.000000000000000000, 0.8176092056337987968, 1.000000000000000000),
 ( 1.000000000000000000, 0.8122961334888495477, 1.000000000000000000),
 ( 1.000000000000000000, 0.8086310951056294716, 1.000000000000000000),
 ( 1.000000000000000000, 0.8047712311394933371, 1.000000000000000000) ) ) 
 REPRESENTATION_ITEM ( '' )  SURFACE ( )  );
#1073 = DIRECTION ( 'NONE',  ( -1.000000000000000000, -0.000000000000000000, -0.000000000000000000 ) ) ;
#1074 = CARTESIAN_POINT ( 'NONE',  ( -25.00000000000000000, 610.0000000000000000, 24.99999999999999645 ) ) ;
#1075 = VERTEX_POINT ( 'NONE', #5044 ) ;
#1076 = AXIS2_PLACEMENT_3D ( 'NONE', #3029, #3003, #101 ) ;
#1077 = ORIENTED_EDGE ( 'NONE', *, *, #894, .T. ) ;
#1078 = VECTOR ( 'NONE', #189, 1000.000000000000000 ) ;
#1079 = ORIENTED_EDGE ( 'NONE', *, *, #1395, .T. ) ;
#1080 = DIRECTION ( 'NONE',  ( 0.000000000000000000, 0.000000000000000000, -1.000000000000000000 ) ) ;
#1081 = EDGE_CURVE ( 'NONE', #4871, #529, #4303, .T. ) ;
#1082 = DIRECTION ( 'NONE',  ( -1.000000000000000000, -0.000000000000000000, -0.000000000000000000 ) ) ;
#1083 = DIRECTION ( 'NONE',  ( 0.000000000000000000, 1.000000000000000000, 0.000000000000000000 ) ) ;
#1084 = CIRCLE ( 'NONE', #4472, 0.9279820837131848021 ) ;
#1085 = ADVANCED_FACE ( 'NONE', ( #5203 ), #3984, .T. ) ;
#1086 = ORIENTED_EDGE ( 'NONE', *, *, #4012, .F. ) ;
#1087 = CARTESIAN_POINT ( 'NONE',  ( 0.6000000000000033085, 0.000000000000000000, 0.000000000000000000 ) ) ;
#1088 = DIRECTION ( 'NONE',  ( 0.000000000000000000, 0.000000000000000000, 1.000000000000000000 ) ) ;
#1089 = FACE_OUTER_BOUND ( 'NONE', #4892, .T. ) ;
#1090 = DIRECTION ( 'NONE',  ( 1.000000000000000000, 0.000000000000000000, 0.000000000000000000 ) ) ;
#1091 = APPLICATION_PROTOCOL_DEFINITION ( 'draft international standard', 'automotive_design', 1998, #4958 ) ;
#1092 = PRODUCT_DEFINITION_FORMATION_WITH_SPECIFIED_SOURCE ( 'ANY', '', #4530, .NOT_KNOWN. ) ;
#1093 = VECTOR ( 'NONE', #4947, 1000.000000000000000 ) ;
#1094 = VERTEX_POINT ( 'NONE', #1114 ) ;
#1095 = ORIENTED_EDGE ( 'NONE', *, *, #380, .F. ) ;
#1096 = CARTESIAN_POINT ( 'NONE',  ( 0.000000000000000000, 810.0000000000000000, -6.000000000000000000 ) ) ;
#1097 = DIRECTION ( 'NONE',  ( 1.000000000000000000, 0.000000000000000000, 0.000000000000000000 ) ) ;
#1098 = DIRECTION ( 'NONE',  ( 0.000000000000000000, 0.000000000000000000, -1.000000000000000000 ) ) ;
#1099 = DIRECTION ( 'NONE',  ( 0.000000000000000000, -0.000000000000000000, 1.000000000000000000 ) ) ;
#1100 = CARTESIAN_POINT ( 'NONE',  ( -9.000000000000000000, -5.196152422706635576, -9.106320693283315393 ) ) ;
#1101 = AXIS2_PLACEMENT_3D ( 'NONE', #1578, #5333, #3322 ) ;
#1102 = EDGE_CURVE ( 'NONE', #4507, #850, #2281, .T. ) ;
#1103 = VECTOR ( 'NONE', #2269, 999.9999999999998863 ) ;
#1104 = FACE_OUTER_BOUND ( 'NONE', #5003, .T. ) ;
#1105 = FACE_OUTER_BOUND ( 'NONE', #71, .T. ) ;
#1106 = EDGE_CURVE ( 'NONE', #3488, #2372, #158, .T. ) ;
#1107 = AXIS2_PLACEMENT_3D ( 'NONE', #3670, #2761, #1088 ) ;
#1108 = ORIENTED_EDGE ( 'NONE', *, *, #79, .F. ) ;
#1109 = EDGE_CURVE ( 'NONE', #3821, #4454, #1453, .T. ) ;
#1110 = VECTOR ( 'NONE', #22, 1000.000000000000000 ) ;
#1111 = ORIENTED_EDGE ( 'NONE', *, *, #2237, .T. ) ;
#1112 = DIRECTION ( 'NONE',  ( 1.000000000000000000, 0.000000000000000000, 0.000000000000000000 ) ) ;
#1113 = VERTEX_POINT ( 'NONE', #616 ) ;
#1114 = CARTESIAN_POINT ( 'NONE',  ( -9.473745496805529243, -1.478735707944909295E-13, -9.138786188337405747 ) ) ;
#1115 = CARTESIAN_POINT ( 'NONE',  ( 0.000000000000000000, 0.000000000000000000, -12.00000000000000000 ) ) ;
#1116 = AXIS2_PLACEMENT_3D ( 'NONE', #2685, #1433, #649 ) ;
#1117 = ORIENTED_EDGE ( 'NONE', *, *, #39, .T. ) ;
#1118 = DIRECTION ( 'NONE',  ( 1.000000000000000000, 0.000000000000000000, 0.000000000000000000 ) ) ;
#1119 = CARTESIAN_POINT ( 'NONE',  ( -7.990639863761101580, -6.344566044901012170, -9.361164777500285084 ) ) ;
#1120 = CARTESIAN_POINT ( 'NONE',  ( 9.489595936502764673, 3.666866907830382161, -9.379652974972602308 ) ) ;
#1121 = DIRECTION ( 'NONE',  ( -1.000000000000000000, -0.000000000000000000, -0.000000000000000000 ) ) ;
#1122 = UNCERTAINTY_MEASURE_WITH_UNIT (LENGTH_MEASURE( 1.000000000000000082E-05 ), #3066, 'distance_accuracy_value', 'NONE');
#1123 = ORIENTED_EDGE ( 'NONE', *, *, #5224, .F. ) ;
#1124 = EDGE_LOOP ( 'NONE', ( #2187, #2700, #3235, #525 ) ) ;
#1125 = PLANE ( 'NONE',  #3717 ) ;
#1126 = CARTESIAN_POINT ( 'NONE',  ( -5.036000000000011134, 570.0000000000000000, -24.99999999999998579 ) ) ;
#1127 = CARTESIAN_POINT ( 'NONE',  ( 0.000000000000000000, 0.000000000000000000, 25.00000000000000000 ) ) ;
#1128 = EDGE_CURVE ( 'NONE', #5301, #2252, #4141, .T. ) ;
#1129 = DIRECTION ( 'NONE',  ( -6.938893903907228378E-17, 0.000000000000000000, 1.000000000000000000 ) ) ;
#1130 = CARTESIAN_POINT ( 'NONE',  ( 6.000000000000000000, -2.919948986426526893, 5.057500000000001883 ) ) ;
#1131 = AXIS2_PLACEMENT_3D ( 'NONE', #251, #4391, #657 ) ;
#1132 = CYLINDRICAL_SURFACE ( 'NONE', #4647, 15.00000000000000000 ) ;
#1133 = CARTESIAN_POINT ( 'NONE',  ( 9.000000000000000000, 1.732050807568874529, -8.505011083697297636 ) ) ;
#1134 =( NAMED_UNIT ( * ) SI_UNIT ( $, .STERADIAN. ) SOLID_ANGLE_UNIT ( ) );
#1135 = ORIENTED_EDGE ( 'NONE', *, *, #5039, .F. ) ;
#1136 = EDGE_CURVE ( 'NONE', #2556, #2061, #2486, .T. ) ;
#1137 = EDGE_LOOP ( 'NONE', ( #2340, #4405, #654, #2970 ) ) ;
#1138 = PLANE ( 'NONE',  #734 ) ;
#1139 = B_SPLINE_CURVE_WITH_KNOTS ( 'NONE', 3,
 ( #166, #214, #4700, #4679, #3959, #4310 ),
 .UNSPECIFIED., .F., .F.,
 ( 4, 2, 4 ),
 ( 0.000000000000000000, 0.0005027859236379887426, 0.001005571847275977485 ),
 .UNSPECIFIED. ) ;
#1140 = DIRECTION ( 'NONE',  ( 0.000000000000000000, -0.000000000000000000, -1.000000000000000000 ) ) ;
#1141 = ORIENTED_EDGE ( 'NONE', *, *, #3126, .T. ) ;
#1142 = ORIENTED_EDGE ( 'NONE', *, *, #1592, .T. ) ;
#1143 = LINE ( 'NONE', #2909, #1406 ) ;
#1144 = CARTESIAN_POINT ( 'NONE',  ( -0.4650146599150260518, -10.12382850633293430, -9.367146555587614998 ) ) ;
#1145 = CARTESIAN_POINT ( 'NONE',  ( -139.9999999999999716, 810.0000000000000000, 25.00000000000000000 ) ) ;
#1146 = DIRECTION ( 'NONE',  ( -1.000000000000000000, -0.000000000000000000, -0.000000000000000000 ) ) ;
#1147 = VERTEX_POINT ( 'NONE', #2311 ) ;
#1148 = AXIS2_PLACEMENT_3D ( 'NONE', #1996, #2445, #4184 ) ;
#1149 = CARTESIAN_POINT ( 'NONE',  ( 75.00000000000000000, 582.4999999999997726, 50.00000000000001421 ) ) ;
#1150 = ORIENTED_EDGE ( 'NONE', *, *, #179, .F. ) ;
#1151 = CARTESIAN_POINT ( 'NONE',  ( -164.0360000000000014, 870.0000000000000000, 6.000000000000006217 ) ) ;
#1152 = FILL_AREA_STYLE ('',( #1522 ) ) ;
#1153 = DIRECTION ( 'NONE',  ( -2.081668171172168513E-16, 0.000000000000000000, 1.000000000000000000 ) ) ;
#1154 = EDGE_CURVE ( 'NONE', #2898, #3300, #2654, .T. ) ;
#1155 = CARTESIAN_POINT ( 'NONE',  ( -150.0000000000000000, 870.0000000000000000, 0.000000000000000000 ) ) ;
#1156 = APPLICATION_CONTEXT ( 'automotive_design' ) ;
#1157 = ORIENTED_EDGE ( 'NONE', *, *, #2641, .T. ) ;
#1158 = FACE_OUTER_BOUND ( 'NONE', #3100, .T. ) ;
#1159 = CARTESIAN_POINT ( 'NONE',  ( 9.000000000000000000, -3.464101615137758383, -8.667800885990210702 ) ) ;
#1160 = VERTEX_POINT ( 'NONE', #1839 ) ;
#1161 = ORIENTED_EDGE ( 'NONE', *, *, #5139, .T. ) ;
#1162 = EDGE_LOOP ( 'NONE', ( #5302, #1244, #3693 ) ) ;
#1163 = B_SPLINE_CURVE_WITH_KNOTS ( 'NONE', 3,
 ( #209, #4811, #5177, #3579, #711, #2347 ),
 .UNSPECIFIED., .F., .F.,
 ( 4, 2, 4 ),
 ( -5.636559625666591986E-06, 0.0004989239064927796776, 0.001003484372611225962 ),
 .UNSPECIFIED. ) ;
#1164 = ORIENTED_EDGE ( 'NONE', *, *, #5118, .T. ) ;
#1165 = FACE_OUTER_BOUND ( 'NONE', #2433, .T. ) ;
#1166 = AXIS2_PLACEMENT_3D ( 'NONE', #1842, #297, #2681 ) ;
#1167 = ORIENTED_EDGE ( 'NONE', *, *, #521, .T. ) ;
#1168 =( NAMED_UNIT ( * ) SI_UNIT ( $, .STERADIAN. ) SOLID_ANGLE_UNIT ( ) );
#1169 = EDGE_CURVE ( 'NONE', #4363, #3498, #2834, .T. ) ;
#1170 = AXIS2_PLACEMENT_3D ( 'NONE', #1540, #292, #4434 ) ;
#1171 = ORIENTED_EDGE ( 'NONE', *, *, #4109, .F. ) ;
#1172 = FACE_OUTER_BOUND ( 'NONE', #3180, .T. ) ;
#1173 = CARTESIAN_POINT ( 'NONE',  ( -6.209422225667362127, -6.807293251912172494, -8.465119797811233582 ) ) ;
#1174 = DIRECTION ( 'NONE',  ( 1.000000000000000000, 0.000000000000000000, -0.000000000000000000 ) ) ;
#1175 = DIRECTION ( 'NONE',  ( 0.000000000000000000, 0.000000000000000000, 1.000000000000000000 ) ) ;
#1176 = APPLICATION_PROTOCOL_DEFINITION ( 'draft international standard', 'automotive_design', 1998, #1156 ) ;
#1177 = EDGE_CURVE ( 'NONE', #3466, #2814, #2395, .T. ) ;
#1178 = AXIS2_PLACEMENT_3D ( 'NONE', #50, #2614, #2635 ) ;
#1179 = DIRECTION ( 'NONE',  ( -1.000000000000000000, -0.000000000000000000, -0.000000000000000000 ) ) ;
#1180 = LINE ( 'NONE', #3703, #3599 ) ;
#1181 = DIRECTION ( 'NONE',  ( 1.000000000000000000, 0.000000000000000000, 0.000000000000000000 ) ) ;
#1182 = PRODUCT_DEFINITION_CONTEXT ( 'detailed design', #4958, 'design' ) ;
#1183 = CARTESIAN_POINT ( 'NONE',  ( -9.000000000000000000, -5.196152422706636465, -8.935996291721336249 ) ) ;
#1184 = AXIS2_PLACEMENT_3D ( 'NONE', #4858, #2059, #4475 ) ;
#1185 = MECHANICAL_DESIGN_GEOMETRIC_PRESENTATION_REPRESENTATION (  '', ( #910 ), #2945 ) ;
#1186 = ADVANCED_FACE ( 'NONE', ( #3897 ), #199, .T. ) ;
#1187 = EDGE_LOOP ( 'NONE', ( #4986, #3605, #643, #4589 ) ) ;
#1188 = CONICAL_SURFACE ( 'NONE', #1866, 12.38940648156203927, 1.221730476396048370 ) ;
#1189 = EDGE_LOOP ( 'NONE', ( #3290, #4950 ) ) ;
#1190 = MECHANICAL_DESIGN_GEOMETRIC_PRESENTATION_REPRESENTATION (  '', ( #2669 ), #3462 ) ;
#1191 = CARTESIAN_POINT ( 'NONE',  ( -165.0000000000000000, 870.0000000000000000, 0.000000000000000000 ) ) ;
#1192 = LINE ( 'NONE', #4977, #3207 ) ;
#1193 = EDGE_CURVE ( 'NONE', #1510, #1969, #3155, .T. ) ;
#1194 = ORIENTED_EDGE ( 'NONE', *, *, #2265, .T. ) ;
#1195 = VERTEX_POINT ( 'NONE', #1817 ) ;
#1196 = VERTEX_POINT ( 'NONE', #1862 ) ;
#1197 = CIRCLE ( 'NONE', #920, 9.000000000000001776 ) ;
#1198 = AXIS2_PLACEMENT_3D ( 'NONE', #4846, #4128, #332 ) ;
#1199 = CARTESIAN_POINT ( 'NONE',  ( 30.00000000000000355, 10.00000000000000000, -30.00000000000000355 ) ) ;
#1200 = EDGE_LOOP ( 'NONE', ( #2737, #2902, #4173, #4013 ) ) ;
#1201 = CIRCLE ( 'NONE', #2515, 6.499999999999988454 ) ;
#1202 = EDGE_CURVE ( 'NONE', #539, #4595, #3574, .T. ) ;
#1203 =( NAMED_UNIT ( * ) PLANE_ANGLE_UNIT ( ) SI_UNIT ( $, .RADIAN. ) );
#1204 = VERTEX_POINT ( 'NONE', #1393 ) ;
#1205 = PLANE ( 'NONE',  #4466 ) ;
#1206 = LINE ( 'NONE', #2980, #232 ) ;
#1207 = DIRECTION ( 'NONE',  ( 0.000000000000000000, 0.000000000000000000, -1.000000000000000000 ) ) ;
#1208 = CARTESIAN_POINT ( 'NONE',  ( 165.0000000000000000, 870.0000000000000000, -6.000000000000001776 ) ) ;
#1209 = VECTOR ( 'NONE', #311, 1000.000000000000000 ) ;
#1210 = PRODUCT_CONTEXT ( 'NONE', #2066, 'mechanical' ) ;
#1211 = VECTOR ( 'NONE', #2256, 1000.000000000000000 ) ;
#1212 = EDGE_CURVE ( 'NONE', #4428, #4561, #3545, .T. ) ;
#1213 = DIRECTION ( 'NONE',  ( 0.000000000000000000, -1.000000000000000000, 0.000000000000000000 ) ) ;
#1214 = ORIENTED_EDGE ( 'NONE', *, *, #2467, .F. ) ;
#1215 = FACE_BOUND ( 'NONE', #3739, .T. ) ;
#1216 = CARTESIAN_POINT ( 'NONE',  ( 25.00000000000000000, 210.0000000000000284, 25.00000000000000711 ) ) ;
#1217 = CARTESIAN_POINT ( 'NONE',  ( 0.000000000000000000, 0.000000000000000000, -12.00000000000000178 ) ) ;
#1218 = EDGE_CURVE ( 'NONE', #4553, #3240, #5228, .T. ) ;
#1219 = CARTESIAN_POINT ( 'NONE',  ( 3.936978610624179531, 8.666338374798533195, -9.138972935415379695 ) ) ;
#1220 = ORIENTED_EDGE ( 'NONE', *, *, #1722, .F. ) ;
#1221 = ORIENTED_EDGE ( 'NONE', *, *, #328, .T. ) ;
#1222 = CARTESIAN_POINT ( 'NONE',  ( 9.506737344437272696, 5.488717364925924436, -9.686084310752812954 ) ) ;
#1223 = DIRECTION ( 'NONE',  ( 0.000000000000000000, 0.000000000000000000, 1.000000000000000000 ) ) ;
#1224 = VERTEX_POINT ( 'NONE', #3925 ) ;
#1225 = VERTEX_POINT ( 'NONE', #1421 ) ;
#1226 = CARTESIAN_POINT ( 'NONE',  ( 6.000000000000000000, 0.000000000000000000, 0.000000000000000000 ) ) ;
#1227 = EDGE_LOOP ( 'NONE', ( #3360, #5032, #123 ) ) ;
#1228 = SHAPE_REPRESENTATION_RELATIONSHIP ( 'NONE' , 'NONE' ,  #1065, #4286 ) ;
#1229 = PRODUCT_RELATED_PRODUCT_CATEGORY ( 'part', '', ( #4530 ) ) ;
#1230 = ORIENTED_EDGE ( 'NONE', *, *, #2338, .F. ) ;
#1231 = FACE_OUTER_BOUND ( 'NONE', #3832, .T. ) ;
#1232 = CARTESIAN_POINT ( 'NONE',  ( 137.5000000000000000, 870.0000000000000000, 0.000000000000000000 ) ) ;
#1233 = PLANE ( 'NONE',  #1011 ) ;
#1234 = CARTESIAN_POINT ( 'NONE',  ( -9.000000000000003553, -1.784038208492157329, -0.1183376658062878922 ) ) ;
#1235 = ITEM_DEFINED_TRANSFORMATION ( 'NONE', 'NONE', #2131,  #4154 ) ;
#1236 = CARTESIAN_POINT ( 'NONE',  ( 5.999999999999988454, 570.0000000000000000, 30.00000000000001066 ) ) ;
#1237 = ORIENTED_EDGE ( 'NONE', *, *, #1632, .F. ) ;
#1238 = CARTESIAN_POINT ( 'NONE',  ( 0.000000000000000000, 0.000000000000000000, 8.400000000000000355 ) ) ;
#1239 = DIRECTION ( 'NONE',  ( 0.000000000000000000, 0.000000000000000000, 1.000000000000000000 ) ) ;
#1240 = CARTESIAN_POINT ( 'NONE',  ( -9.000000000000000000, 3.843049336495677260, -8.684764317652872379 ) ) ;
#1241 = EDGE_CURVE ( 'NONE', #4454, #966, #3104, .T. ) ;
#1242 = PLANE ( 'NONE',  #54 ) ;
#1243 = DIRECTION ( 'NONE',  ( -0.000000000000000000, -0.000000000000000000, -1.000000000000000000 ) ) ;
#1244 = ORIENTED_EDGE ( 'NONE', *, *, #937, .F. ) ;
#1245 = ORIENTED_EDGE ( 'NONE', *, *, #4608, .T. ) ;
#1246 = CARTESIAN_POINT ( 'NONE',  ( 0.000000000000000000, 330.0000000000000000, 25.00000000000000000 ) ) ;
#1247 = ORIENTED_EDGE ( 'NONE', *, *, #2005, .T. ) ;
#1248 = EDGE_CURVE ( 'NONE', #503, #3980, #2343, .T. ) ;
#1249 = EDGE_LOOP ( 'NONE', ( #767, #2867, #5272, #681 ) ) ;
#1250 = DIRECTION ( 'NONE',  ( 0.000000000000000000, 0.000000000000000000, 1.000000000000000000 ) ) ;
#1251 = DIRECTION ( 'NONE',  ( -0.000000000000000000, -1.000000000000000000, -0.000000000000000000 ) ) ;
#1252 = CARTESIAN_POINT ( 'NONE',  ( -0.05527946870650939093, -11.01006727514132066, -9.698012095152312995 ) ) ;
#1253 = EDGE_CURVE ( 'NONE', #81, #3733, #3960, .T. ) ;
#1254 = CONICAL_SURFACE ( 'NONE', #3167, 5.036000000000040444, 0.7853981633974339571 ) ;
#1255 = AXIS2_PLACEMENT_3D ( 'NONE', #5258, #239, #2255 ) ;
#1256 = PLANE ( 'NONE',  #1449 ) ;
#1257 = PRESENTATION_STYLE_ASSIGNMENT (( #1643 ) ) ;
#1258 = DIRECTION ( 'NONE',  ( 0.000000000000000000, 0.000000000000000000, 1.000000000000000000 ) ) ;
#1259 = LINE ( 'NONE', #3374, #1983 ) ;
#1260 = SHAPE_REPRESENTATION_RELATIONSHIP ( 'NONE' , 'NONE' ,  #121, #2208 ) ;
#1261 = CONICAL_SURFACE ( 'NONE', #5087, 5.999999999999993783, 0.7853981633974491672 ) ;
#1262 = ORIENTED_EDGE ( 'NONE', *, *, #2641, .F. ) ;
#1263 = ORIENTED_EDGE ( 'NONE', *, *, #3700, .T. ) ;
#1264 = CARTESIAN_POINT ( 'NONE',  ( 9.000000000000000000, 5.196152422706629359, -12.00000000000000000 ) ) ;
#1265 = CARTESIAN_POINT ( 'NONE',  ( -1.676835913137321903E-15, 35.00000000000000000, -25.00000000000000000 ) ) ;
#1266 = STYLED_ITEM ( 'NONE', ( #556 ), #5266 ) ;
#1267 = ORIENTED_EDGE ( 'NONE', *, *, #2794, .T. ) ;
#1268 = ORIENTED_EDGE ( 'NONE', *, *, #1102, .F. ) ;
#1269 = CARTESIAN_POINT ( 'NONE',  ( 8.999999999999998224, -1.732050807568880968, -8.505011083697294083 ) ) ;
#1270 = CIRCLE ( 'NONE', #1184, 6.000000000000006217 ) ;
#1271 = DIRECTION ( 'NONE',  ( -0.000000000000000000, -1.000000000000000000, -0.000000000000000000 ) ) ;
#1272 = ADVANCED_FACE ( 'NONE', ( #4042 ), #3632, .T. ) ;
#1273 = ORIENTED_EDGE ( 'NONE', *, *, #1106, .T. ) ;
#1274 = EDGE_LOOP ( 'NONE', ( #1059, #1123, #2107, #2096 ) ) ;
#1275 = ADVANCED_FACE ( 'NONE', ( #5288, #4865 ), #1138, .T. ) ;
#1276 = AXIS2_PLACEMENT_3D ( 'NONE', #4113, #3259, #721 ) ;
#1277 = STYLED_ITEM ( 'NONE', ( #4776 ), #387 ) ;
#1278 = VECTOR ( 'NONE', #1829, 1000.000000000000000 ) ;
#1279 = VERTEX_POINT ( 'NONE', #2369 ) ;
#1280 = FACE_BOUND ( 'NONE', #2660, .T. ) ;
#1281 = CARTESIAN_POINT ( 'NONE',  ( 9.000000000000001776, -5.196152422706638241, -1.199999999999999734 ) ) ;
#1282 = FACE_OUTER_BOUND ( 'NONE', #2645, .T. ) ;
#1283 = AXIS2_PLACEMENT_3D ( 'NONE', #3128, #4799, #3416 ) ;
#1284 = DIRECTION ( 'NONE',  ( 1.000000000000000000, 0.000000000000000000, -0.000000000000000000 ) ) ;
#1285 = ORIENTED_EDGE ( 'NONE', *, *, #3872, .F. ) ;
#1286 = DIRECTION ( 'NONE',  ( 0.000000000000000000, 0.000000000000000000, -1.000000000000000000 ) ) ;
#1287 = CARTESIAN_POINT ( 'NONE',  ( -3.715604115503467142, -8.247099809125261416, -0.03002505116510541944 ) ) ;
#1288 = VECTOR ( 'NONE', #2476, 1000.000000000000000 ) ;
#1289 = DIRECTION ( 'NONE',  ( 0.000000000000000000, 1.000000000000000000, -1.188187522481193495E-15 ) ) ;
#1290 = CARTESIAN_POINT ( 'NONE',  ( -8.999999999999998224, 1.936561697304590934, -8.969347964766754444 ) ) ;
#1291 = AXIS2_PLACEMENT_3D ( 'NONE', #1570, #4441, #3252 ) ;
#1292 = EDGE_CURVE ( 'NONE', #165, #2065, #2179, .T. ) ;
#1293 = ORIENTED_EDGE ( 'NONE', *, *, #4109, .T. ) ;
#1294 = ORIENTED_EDGE ( 'NONE', *, *, #4878, .T. ) ;
#1295 = CARTESIAN_POINT ( 'NONE',  ( 0.4650146599169583395, 10.12382850633530751, -9.367146555589735968 ) ) ;
#1296 = CARTESIAN_POINT ( 'NONE',  ( 6.332118058842089781, -7.287734290476359789, -9.190020220263406259 ) ) ;
#1297 = ORIENTED_EDGE ( 'NONE', *, *, #2518, .F. ) ;
#1298 = ORIENTED_EDGE ( 'NONE', *, *, #4429, .T. ) ;
#1299 = CARTESIAN_POINT ( 'NONE',  ( 121.7157287525372311, -20.00000000000000000, -121.7157287525388369 ) ) ;
#1300 = ADVANCED_FACE ( 'NONE', ( #4202 ), #3875, .T. ) ;
#1301 = EDGE_CURVE ( 'NONE', #338, #2174, #3008, .T. ) ;
#1302 = ORIENTED_EDGE ( 'NONE', *, *, #3286, .F. ) ;
#1303 = DIRECTION ( 'NONE',  ( -0.7071067811865291430, 0.000000000000000000, 0.7071067811865660024 ) ) ;
#1304 = PLANE ( 'NONE',  #3654 ) ;
#1305 = DIRECTION ( 'NONE',  ( 1.000000000000000000, 0.000000000000000000, 0.000000000000000000 ) ) ;
#1306 = CARTESIAN_POINT ( 'NONE',  ( -9.000000000000000000, 1.123146974283612654, -0.05788585198792847025 ) ) ;
#1307 = EDGE_LOOP ( 'NONE', ( #4818, #5283 ) ) ;
#1308 = DIRECTION ( 'NONE',  ( 1.000000000000000000, -0.000000000000000000, 2.081668171172168513E-16 ) ) ;
#1309 = CARTESIAN_POINT ( 'NONE',  ( -2.569563281917990771, -8.908766792898138220, -0.2264046624879807734 ) ) ;
#1310 = CARTESIAN_POINT ( 'NONE',  ( -6.245004513516506329E-15, 610.0000000000000000, 30.00000000000000711 ) ) ;
#1311 = CARTESIAN_POINT ( 'NONE',  ( -9.473946373357962969, 1.923623857792322145, -9.141672110797713913 ) ) ;
#1312 =( NAMED_UNIT ( * ) SI_UNIT ( $, .STERADIAN. ) SOLID_ANGLE_UNIT ( ) );
#1313 = ADVANCED_FACE ( 'NONE', ( #5047 ), #462, .T. ) ;
#1314 = ORIENTED_EDGE ( 'NONE', *, *, #1686, .T. ) ;
#1315 = ADVANCED_FACE ( 'NONE', ( #4622, #2153 ), #438, .T. ) ;
#1316 = CARTESIAN_POINT ( 'NONE',  ( -150.0000000000000000, 870.0000000000000000, 0.000000000000000000 ) ) ;
#1317 = DIRECTION ( 'NONE',  ( 1.000000000000000000, 0.000000000000000000, 0.000000000000000000 ) ) ;
#1318 = FACE_OUTER_BOUND ( 'NONE', #4015, .T. ) ;
#1319 = ORIENTED_EDGE ( 'NONE', *, *, #908, .F. ) ;
#1320 = CYLINDRICAL_SURFACE ( 'NONE', #3962, 15.00000000000000000 ) ;
#1321 = CYLINDRICAL_SURFACE ( 'NONE', #1076, 6.000000000000001776 ) ;
#1322 = ADVANCED_FACE ( 'NONE', ( #5098 ), #987, .F. ) ;
#1323 = LINE ( 'NONE', #4743, #2686 ) ;
#1324 = CARTESIAN_POINT ( 'NONE',  ( -9.000000000000000000, -4.368650009232622367, -0.8589767385557532942 ) ) ;
#1325 = AXIS2_PLACEMENT_3D ( 'NONE', #3342, #2525, #5331 ) ;
#1326 = CARTESIAN_POINT ( 'NONE',  ( 12.00000000000000000, 0.000000000000000000, 0.000000000000000000 ) ) ;
#1327 = CARTESIAN_POINT ( 'NONE',  ( 9.473745496805529243, 1.478328004173170497E-13, -9.138786188337405747 ) ) ;
#1328 = CARTESIAN_POINT ( 'NONE',  ( 11.99999999999999645, 0.000000000000000000, 0.000000000000000000 ) ) ;
#1329 = DIRECTION ( 'NONE',  ( -0.000000000000000000, -0.000000000000000000, 1.000000000000000000 ) ) ;
#1330 = ORIENTED_EDGE ( 'NONE', *, *, #4981, .F. ) ;
#1331 = ADVANCED_FACE ( 'NONE', ( #877 ), #1376, .F. ) ;
#1332 = CARTESIAN_POINT ( 'NONE',  ( -9.000000000000000000, -4.737975421414065913, -8.849003814629385900 ) ) ;
#1333 = AXIS2_PLACEMENT_3D ( 'NONE', #3641, #821, #2462 ) ;
#1334 = VECTOR ( 'NONE', #3501, 1000.000000000000000 ) ;
#1335 = ORIENTED_EDGE ( 'NONE', *, *, #2449, .T. ) ;
#1336 = PRESENTATION_STYLE_ASSIGNMENT (( #2164 ) ) ;
#1337 = CARTESIAN_POINT ( 'NONE',  ( 3.145560420647533828, 9.127459525684209041, -9.189462574975609144 ) ) ;
#1338 = CARTESIAN_POINT ( 'NONE',  ( 121.7157287525384533, 0.000000000000000000, 106.7157287525376859 ) ) ;
#1339 = EDGE_LOOP ( 'NONE', ( #2416, #2759, #4548, #5314 ) ) ;
#1340 = CIRCLE ( 'NONE', #2041, 6.499999999999988454 ) ;
#1341 = EDGE_CURVE ( 'NONE', #3771, #2114, #4674, .T. ) ;
#1342 = CARTESIAN_POINT ( 'NONE',  ( -5.099999999999999645, 6.245698675651500839E-16, -12.00000000000000000 ) ) ;
#1343 =( NAMED_UNIT ( * ) SI_UNIT ( $, .STERADIAN. ) SOLID_ANGLE_UNIT ( ) );
#1344 = AXIS2_PLACEMENT_3D ( 'NONE', #3711, #3210, #3301 ) ;
#1345 = MECHANICAL_DESIGN_GEOMETRIC_PRESENTATION_REPRESENTATION (  '', ( #1266 ), #5013 ) ;
#1346 = ORIENTED_EDGE ( 'NONE', *, *, #2543, .F. ) ;
#1347 = ADVANCED_FACE ( 'NONE', ( #3055, #496 ), #2097, .F. ) ;
#1348 = DIRECTION ( 'NONE',  ( -0.000000000000000000, -1.000000000000000000, -0.000000000000000000 ) ) ;
#1349 = CIRCLE ( 'NONE', #753, 5.035999999999999588 ) ;
#1350 = ORIENTED_EDGE ( 'NONE', *, *, #391, .F. ) ;
#1351 = DIRECTION ( 'NONE',  ( 0.000000000000000000, 0.000000000000000000, -1.000000000000000000 ) ) ;
#1352 = AXIS2_PLACEMENT_3D ( 'NONE', #3909, #5180, #3583 ) ;
#1353 = CARTESIAN_POINT ( 'NONE',  ( 5.035999999999988042, 570.0000000000000000, -24.99999999999998579 ) ) ;
#1354 = PRODUCT_DEFINITION_SHAPE ( 'NONE', 'NONE',  #979 ) ;
#1355 = CIRCLE ( 'NONE', #2063, 6.499999999999988454 ) ;
#1356 = DIRECTION ( 'NONE',  ( 0.000000000000000000, -0.000000000000000000, -1.000000000000000000 ) ) ;
#1357 = ORIENTED_EDGE ( 'NONE', *, *, #4166, .F. ) ;
#1358 = DIRECTION ( 'NONE',  ( -1.000000000000000000, 0.000000000000000000, 0.000000000000000000 ) ) ;
#1359 = CARTESIAN_POINT ( 'NONE',  ( -139.9999999999999716, 870.0000000000000000, 5.999999999999950262 ) ) ;
#1360 = CARTESIAN_POINT ( 'NONE',  ( 0.000000000000000000, 330.0000000000000000, -25.00000000000000000 ) ) ;
#1361 = VECTOR ( 'NONE', #3225, 1000.000000000000000 ) ;
#1362 = EDGE_CURVE ( 'NONE', #3765, #754, #3791, .T. ) ;
#1363 = ADVANCED_FACE ( 'NONE', ( #3441 ), #383, .F. ) ;
#1364 = CARTESIAN_POINT ( 'NONE',  ( 12.59999999999999964, 0.000000000000000000, 0.000000000000000000 ) ) ;
#1365 = CARTESIAN_POINT ( 'NONE',  ( 92.00000000000000000, 6.167321280506070407E-16, -5.035999999999999588 ) ) ;
#1366 = DIRECTION ( 'NONE',  ( -1.000000000000000000, 0.000000000000000000, 0.000000000000000000 ) ) ;
#1367 = CARTESIAN_POINT ( 'NONE',  ( 6.209422225666635597, 6.807293251912587273, -8.465119797812908686 ) ) ;
#1368 = CARTESIAN_POINT ( 'NONE',  ( 7.347880794884119736E-16, 810.0000000000000000, 6.000000000000000000 ) ) ;
#1369 = CIRCLE ( 'NONE', #4508, 6.499999999999988454 ) ;
#1370 = LINE ( 'NONE', #1734, #5092 ) ;
#1371 = SURFACE_STYLE_FILL_AREA ( #5086 ) ;
#1372 = EDGE_LOOP ( 'NONE', ( #4478, #589, #4101, #1914 ) ) ;
#1373 = DIRECTION ( 'NONE',  ( -1.000000000000000000, -0.000000000000000000, -0.000000000000000000 ) ) ;
#1374 = DIRECTION ( 'NONE',  ( 6.938893903907228378E-17, 0.000000000000000000, -1.000000000000000000 ) ) ;
#1375 = CARTESIAN_POINT ( 'NONE',  ( -139.9999999999999716, 820.0000000000001137, -25.00000000000000000 ) ) ;
#1376 = PLANE ( 'NONE',  #1851 ) ;
#1377 = EDGE_LOOP ( 'NONE', ( #2702, #5065, #3631, #3686 ) ) ;
#1378 = DIRECTION ( 'NONE',  ( -0.000000000000000000, -1.000000000000000000, -0.000000000000000000 ) ) ;
#1379 = CARTESIAN_POINT ( 'NONE',  ( -150.0000000000000000, 820.0000000000001137, -25.00000000000000000 ) ) ;
#1380 = DIRECTION ( 'NONE',  ( -2.775557561562891351E-16, 0.000000000000000000, 1.000000000000000000 ) ) ;
#1381 = DIRECTION ( 'NONE',  ( 0.000000000000000000, -1.000000000000000000, 0.000000000000000000 ) ) ;
#1382 = CARTESIAN_POINT ( 'NONE',  ( 0.7169666604817516165, -9.978363950984148190, -0.8432325327665534109 ) ) ;
#1383 = CARTESIAN_POINT ( 'NONE',  ( 0.000000000000000000, 570.0000000000000000, 25.00000000000000000 ) ) ;
#1384 = DIRECTION ( 'NONE',  ( 2.081668171172168513E-16, 0.000000000000000000, -1.000000000000000000 ) ) ;
#1385 = LINE ( 'NONE', #582, #1966 ) ;
#1386 = CARTESIAN_POINT ( 'NONE',  ( -6.499999999999988454, 510.0000000000000000, 25.00000000000000000 ) ) ;
#1387 = EDGE_CURVE ( 'NONE', #3047, #1861, #4637, .T. ) ;
#1388 = CARTESIAN_POINT ( 'NONE',  ( -6.499999999999988454, 570.0000000000000000, 25.00000000000000000 ) ) ;
#1389 = ORIENTED_EDGE ( 'NONE', *, *, #1472, .F. ) ;
#1390 = B_SPLINE_CURVE_WITH_KNOTS ( 'NONE', 3,
 ( #2023, #2420, #1579, #1556, #1219, #3261, #2448, #2472, #2859, #4089 ),
 .UNSPECIFIED., .F., .F.,
 ( 4, 2, 2, 2, 4 ),
 ( 0.000000000000000000, 0.002766603965071789701, 0.005533207930143578535, 0.008299811895215367802, 0.01106641586028715707 ),
 .UNSPECIFIED. ) ;
#1391 = EDGE_LOOP ( 'NONE', ( #4455, #5173, #2058, #4539 ) ) ;
#1392 = DIRECTION ( 'NONE',  ( 0.000000000000000000, 0.000000000000000000, -1.000000000000000000 ) ) ;
#1393 = CARTESIAN_POINT ( 'NONE',  ( -6.499999999999984901, 35.00000000000000000, 25.00000000000000000 ) ) ;
#1394 = CARTESIAN_POINT ( 'NONE',  ( -24.99999999999999645, 810.0000000000000000, -25.00000000000000000 ) ) ;
#1395 = EDGE_CURVE ( 'NONE', #4086, #3383, #4755, .T. ) ;
#1396 = ORIENTED_EDGE ( 'NONE', *, *, #453, .F. ) ;
#1397 = VERTEX_POINT ( 'NONE', #2602 ) ;
#1398 = CARTESIAN_POINT ( 'NONE',  ( 6.000000000000000000, -5.839897972853064445, 4.770489558936219510E-15 ) ) ;
#1399 = EDGE_CURVE ( 'NONE', #656, #2372, #5132, .T. ) ;
#1400 = CARTESIAN_POINT ( 'NONE',  ( 6.499999999999988454, 330.0000000000000000, 25.00000000000000000 ) ) ;
#1401 = ORIENTED_EDGE ( 'NONE', *, *, #2128, .T. ) ;
#1402 = CARTESIAN_POINT ( 'NONE',  ( 75.00000000000000000, 582.4999999999997726, 30.00000000000002132 ) ) ;
#1403 = DIRECTION ( 'NONE',  ( 1.000000000000000000, 0.000000000000000000, 0.000000000000000000 ) ) ;
#1404 = ORIENTED_EDGE ( 'NONE', *, *, #3129, .T. ) ;
#1405 = FACE_OUTER_BOUND ( 'NONE', #5287, .T. ) ;
#1406 = VECTOR ( 'NONE', #4542, 1000.000000000000000 ) ;
#1407 = CARTESIAN_POINT ( 'NONE',  ( 30.00000000000000355, 610.0000000000000000, -30.00000000000000355 ) ) ;
#1408 = EDGE_CURVE ( 'NONE', #4400, #1225, #4074, .T. ) ;
#1409 = DIRECTION ( 'NONE',  ( -0.000000000000000000, -0.000000000000000000, 1.000000000000000000 ) ) ;
#1410 = FACE_OUTER_BOUND ( 'NONE', #1249, .T. ) ;
#1411 = CIRCLE ( 'NONE', #5004, 15.00000000000000000 ) ;
#1412 = CARTESIAN_POINT ( 'NONE',  ( 9.000000000000000000, 5.196152422706629359, -8.935996291721334472 ) ) ;
#1413 = LINE ( 'NONE', #2595, #4663 ) ;
#1414 = VECTOR ( 'NONE', #1348, 1000.000000000000000 ) ;
#1415 = CIRCLE ( 'NONE', #3532, 5.999999999999996447 ) ;
#1416 = ADVANCED_FACE ( 'NONE', ( #3065 ), #2212, .F. ) ;
#1417 = EDGE_CURVE ( 'NONE', #81, #963, #3912, .T. ) ;
#1418 = VERTEX_POINT ( 'NONE', #3558 ) ;
#1419 = CARTESIAN_POINT ( 'NONE',  ( 121.7157287525372311, -20.00000000000000000, -121.7157287525388369 ) ) ;
#1420 = EDGE_CURVE ( 'NONE', #5142, #1913, #4815, .T. ) ;
#1421 = CARTESIAN_POINT ( 'NONE',  ( -1.301042606982605321E-14, -10.39230484541326760, -1.199999999999999734 ) ) ;
#1422 = DIRECTION ( 'NONE',  ( -0.000000000000000000, -0.000000000000000000, 1.000000000000000000 ) ) ;
#1423 = AXIS2_PLACEMENT_3D ( 'NONE', #1316, #2995, #2132 ) ;
#1424 = B_SPLINE_CURVE_WITH_KNOTS ( 'NONE', 3,
 ( #4412, #4873, #647, #4439, #3250, #1513 ),
 .UNSPECIFIED., .F., .F.,
 ( 4, 2, 4 ),
 ( 0.005333245961717302495, 0.007986067645924079320, 0.01063888933013085701 ),
 .UNSPECIFIED. ) ;
#1425 = AXIS2_PLACEMENT_3D ( 'NONE', #1666, #2967, #4606 ) ;
#1426 = COLOUR_RGB ( '',1.000000000000000000, 0.9490196078431372140, 0.9098039215686274384 ) ;
#1427 = EDGE_LOOP ( 'NONE', ( #1220, #3769, #1141, #1214 ) ) ;
#1428 = EDGE_LOOP ( 'NONE', ( #3649, #4159, #2102, #844 ) ) ;
#1429 = ORIENTED_EDGE ( 'NONE', *, *, #940, .F. ) ;
#1430 = CARTESIAN_POINT ( 'NONE',  ( -9.000000000000000000, 5.196152422706629359, -1.199999999999997291 ) ) ;
#1431 = CARTESIAN_POINT ( 'NONE',  ( 75.00000000000000000, 582.4999999999997726, 50.00000000000001421 ) ) ;
#1432 = DIRECTION ( 'NONE',  ( 0.000000000000000000, 0.000000000000000000, -1.000000000000000000 ) ) ;
#1433 = DIRECTION ( 'NONE',  ( 0.000000000000000000, 0.000000000000000000, 1.000000000000000000 ) ) ;
#1434 = SURFACE_STYLE_USAGE ( .BOTH. , #3479 ) ;
#1435 = CIRCLE ( 'NONE', #4240, 0.9279820837131848021 ) ;
#1436 = ORIENTED_EDGE ( 'NONE', *, *, #2982, .T. ) ;
#1437 = DIRECTION ( 'NONE',  ( 0.000000000000000000, 0.000000000000000000, -1.000000000000000000 ) ) ;
#1438 = CARTESIAN_POINT ( 'NONE',  ( 150.0000000000000000, 885.0000000000000000, 25.00000000000000000 ) ) ;
#1439 = CARTESIAN_POINT ( 'NONE',  ( -9.000000000000000000, 5.196152422706629359, -12.00000000000000000 ) ) ;
#1440 = CIRCLE ( 'NONE', #3204, 9.000000000000000000 ) ;
#1441 = CARTESIAN_POINT ( 'NONE',  ( 0.000000000000000000, -2.919948986426526893, 5.057500000000001883 ) ) ;
#1442 = DIRECTION ( 'NONE',  ( 0.000000000000000000, 0.000000000000000000, -1.000000000000000000 ) ) ;
#1443 = B_SPLINE_CURVE_WITH_KNOTS ( 'NONE', 3,
 ( #1412, #4742, #425, #4451, #4914, #1222 ),
 .UNSPECIFIED., .F., .F.,
 ( 4, 2, 4 ),
 ( 1.734723475976807094E-18, 0.0005027859236379904773, 0.001005571847275979220 ),
 .UNSPECIFIED. ) ;
#1444 = VECTOR ( 'NONE', #2559, 1000.000000000000000 ) ;
#1445 = LINE ( 'NONE', #1912, #3386 ) ;
#1446 = AXIS2_PLACEMENT_3D ( 'NONE', #573, #5179, #4342 ) ;
#1447 = VERTEX_POINT ( 'NONE', #4703 ) ;
#1448 = AXIS2_PLACEMENT_3D ( 'NONE', #181, #127, #3847 ) ;
#1449 = AXIS2_PLACEMENT_3D ( 'NONE', #339, #4578, #2098 ) ;
#1450 = ORIENTED_EDGE ( 'NONE', *, *, #4120, .F. ) ;
#1451 = CARTESIAN_POINT ( 'NONE',  ( 0.000000000000000000, 0.000000000000000000, 0.000000000000000000 ) ) ;
#1452 = VERTEX_POINT ( 'NONE', #2735 ) ;
#1453 = LINE ( 'NONE', #2226, #3873 ) ;
#1454 = CARTESIAN_POINT ( 'NONE',  ( 0.000000000000000000, 0.000000000000000000, 0.000000000000000000 ) ) ;
#1455 = ADVANCED_FACE ( 'NONE', ( #1803 ), #4560, .T. ) ;
#1456 = ORIENTED_EDGE ( 'NONE', *, *, #742, .T. ) ;
#1457 = VERTEX_POINT ( 'NONE', #4315 ) ;
#1458 = PLANE ( 'NONE',  #4051 ) ;
#1459 = CARTESIAN_POINT ( 'NONE',  ( -1.215778977584765608, -9.690374525429620078, -8.707326526324040472 ) ) ;
#1460 = DIRECTION ( 'NONE',  ( 0.000000000000000000, 0.000000000000000000, -1.000000000000000000 ) ) ;
#1461 = CARTESIAN_POINT ( 'NONE',  ( 149.9999999999999716, 0.000000000000000000, 149.9999999999999716 ) ) ;
#1462 = DIRECTION ( 'NONE',  ( 0.000000000000000000, 0.000000000000000000, 1.000000000000000000 ) ) ;
#1463 = LINE ( 'NONE', #3039, #2746 ) ;
#1464 = ORIENTED_EDGE ( 'NONE', *, *, #1248, .F. ) ;
#1465 =( LENGTH_UNIT ( ) NAMED_UNIT ( * ) SI_UNIT ( .MILLI., .METRE. ) );
#1466 = CARTESIAN_POINT ( 'NONE',  ( -6.000000000000005329, 570.0000000000000000, -24.03599999999999071 ) ) ;
#1467 = DIRECTION ( 'NONE',  ( -1.000000000000000000, -0.000000000000000000, -0.000000000000000000 ) ) ;
#1468 = CARTESIAN_POINT ( 'NONE',  ( 25.00000000000000000, 10.00000000000000000, -25.00000000000000000 ) ) ;
#1469 = EDGE_CURVE ( 'NONE', #3920, #601, #2517, .T. ) ;
#1470 = CARTESIAN_POINT ( 'NONE',  ( 8.999999999999998224, -1.936944919200365156, -8.969396369466336338 ) ) ;
#1471 = DIRECTION ( 'NONE',  ( 1.000000000000000000, 0.000000000000000000, 0.000000000000000000 ) ) ;
#1472 = EDGE_CURVE ( 'NONE', #4918, #3738, #3088, .T. ) ;
#1473 = ORIENTED_EDGE ( 'NONE', *, *, #5184, .T. ) ;
#1474 = ORIENTED_EDGE ( 'NONE', *, *, #2136, .F. ) ;
#1475 = AXIS2_PLACEMENT_3D ( 'NONE', #1383, #4705, #2656 ) ;
#1476 = EDGE_LOOP ( 'NONE', ( #3157, #4991, #5195, #4804 ) ) ;
#1477 = CARTESIAN_POINT ( 'NONE',  ( -5.099999999999999645, 6.245698675651500839E-16, -11.34441321561125626 ) ) ;
#1478 = EDGE_LOOP ( 'NONE', ( #4056, #1960 ) ) ;
#1479 = DIRECTION ( 'NONE',  ( 1.000000000000000000, 0.000000000000000000, 1.850371707708594316E-16 ) ) ;
#1480 = PRODUCT_DEFINITION_SHAPE ( 'NONE', 'NONE',  #5397 ) ;
#1481 = EDGE_CURVE ( 'NONE', #5234, #1794, #578, .T. ) ;
#1482 = ORIENTED_EDGE ( 'NONE', *, *, #2888, .F. ) ;
#1483 = ORIENTED_EDGE ( 'NONE', *, *, #3142, .T. ) ;
#1484 = DIRECTION ( 'NONE',  ( 0.000000000000000000, 0.000000000000000000, 1.000000000000000000 ) ) ;
#1485 = CARTESIAN_POINT ( 'NONE',  ( 0.000000000000000000, 450.0000000000000000, 25.00000000000000000 ) ) ;
#1486 = CARTESIAN_POINT ( 'NONE',  ( 6.000000000000000000, 5.839897972853065333, -6.938893903907228378E-15 ) ) ;
#1487 = DIRECTION ( 'NONE',  ( 1.000000000000000000, 0.000000000000000000, 0.000000000000000000 ) ) ;
#1488 = DIRECTION ( 'NONE',  ( 1.000000000000000000, 0.000000000000000000, 6.123233995736766036E-17 ) ) ;
#1489 = VERTEX_POINT ( 'NONE', #219 ) ;
#1490 = ORIENTED_EDGE ( 'NONE', *, *, #4897, .F. ) ;
#1491 = EDGE_CURVE ( 'NONE', #2868, #3079, #2293, .T. ) ;
#1492 = FACE_OUTER_BOUND ( 'NONE', #346, .T. ) ;
#1493 = PLANE ( 'NONE',  #3592 ) ;
#1494 = CARTESIAN_POINT ( 'NONE',  ( 9.000000000000000000, 5.196152422706629359, -12.00000000000000000 ) ) ;
#1495 = CARTESIAN_POINT ( 'NONE',  ( -150.0000000000000000, 870.0000000000000000, 0.000000000000000000 ) ) ;
#1496 = EDGE_CURVE ( 'NONE', #2213, #4532, #2628, .T. ) ;
#1497 = CARTESIAN_POINT ( 'NONE',  ( 0.000000000000000000, 330.0000000000000000, 25.00000000000000000 ) ) ;
#1498 = FACE_OUTER_BOUND ( 'NONE', #1428, .T. ) ;
#1499 = CYLINDRICAL_SURFACE ( 'NONE', #4583, 15.00000000000000000 ) ;
#1500 = EDGE_CURVE ( 'NONE', #2146, #4714, #1463, .T. ) ;
#1501 = ORIENTED_EDGE ( 'NONE', *, *, #3927, .T. ) ;
#1502 = AXIS2_PLACEMENT_3D ( 'NONE', #4105, #5347, #5379 ) ;
#1503 = AXIS2_PLACEMENT_3D ( 'NONE', #591, #3185, #4780 ) ;
#1504 = CARTESIAN_POINT ( 'NONE',  ( 1.410908427127813464E-14, 582.4999999999997726, 50.00000000000000000 ) ) ;
#1505 = CYLINDRICAL_SURFACE ( 'NONE', #4825, 6.000000000000001776 ) ;
#1506 = ORIENTED_EDGE ( 'NONE', *, *, #1408, .T. ) ;
#1507 = DIRECTION ( 'NONE',  ( 0.000000000000000000, 0.000000000000000000, 1.000000000000000000 ) ) ;
#1508 = CARTESIAN_POINT ( 'NONE',  ( -150.0000000000000000, 810.0000000000000000, 25.00000000000000000 ) ) ;
#1509 = ADVANCED_FACE ( 'NONE', ( #5106, #2689 ), #4345, .F. ) ;
#1510 = VERTEX_POINT ( 'NONE', #5156 ) ;
#1511 = VECTOR ( 'NONE', #78, 1000.000000000000000 ) ;
#1512 = DIRECTION ( 'NONE',  ( -0.000000000000000000, -0.000000000000000000, 1.000000000000000000 ) ) ;
#1513 = CARTESIAN_POINT ( 'NONE',  ( 9.000000000000000000, 5.196152422706636465, -1.199999999999999734 ) ) ;
#1514 = FACE_BOUND ( 'NONE', #4193, .T. ) ;
#1515 = CARTESIAN_POINT ( 'NONE',  ( -9.506737344437272696, -5.488717364925931541, -9.686084310752812954 ) ) ;
#1516 = CARTESIAN_POINT ( 'NONE',  ( 0.000000000000000000, 839.0360000000000582, -5.999999999999996447 ) ) ;
#1517 = AXIS2_PLACEMENT_3D ( 'NONE', #2658, #1099, #3485 ) ;
#1518 = VERTEX_POINT ( 'NONE', #2242 ) ;
#1519 = DIRECTION ( 'NONE',  ( -1.000000000000000000, -0.000000000000000000, -0.000000000000000000 ) ) ;
#1520 = ORIENTED_EDGE ( 'NONE', *, *, #631, .T. ) ;
#1521 = CARTESIAN_POINT ( 'NONE',  ( -5.527857873577812775, -7.747813868291107298, -9.138600484129264956 ) ) ;
#1522 = FILL_AREA_STYLE_COLOUR ( '', #3810 ) ;
#1523 = DIRECTION ( 'NONE',  ( 0.7071067811865482389, 0.000000000000000000, 0.7071067811865469066 ) ) ;
#1524 = CARTESIAN_POINT ( 'NONE',  ( -9.506737344437272696, -5.488717364925931541, -9.686084310752812954 ) ) ;
#1525 = VECTOR ( 'NONE', #2740, 1000.000000000000000 ) ;
#1526 = B_SPLINE_CURVE_WITH_KNOTS ( 'NONE', 3,
 ( #1692, #4265, #4186, #4164, #422, #17, #2554, #1668, #3344 ),
 .UNSPECIFIED., .F., .F.,
 ( 4, 2, 1, 2, 4 ),
 ( 0.000000000000000000, 0.002598076211353316737, 0.005196152422706633474, 0.007794228634059948910, 0.01039230484541326521 ),
 .UNSPECIFIED. ) ;
#1527 = ADVANCED_FACE ( 'NONE', ( #1405 ), #1261, .T. ) ;
#1528 = EDGE_CURVE ( 'NONE', #4480, #539, #3272, .T. ) ;
#1529 = MECHANICAL_DESIGN_GEOMETRIC_PRESENTATION_REPRESENTATION (  '', ( #3380 ), #664 ) ;
#1530 = CARTESIAN_POINT ( 'NONE',  ( -25.00000000000000000, 10.00000000000000000, 25.00000000000000000 ) ) ;
#1531 = CARTESIAN_POINT ( 'NONE',  ( -6.245004513516506329E-15, 557.4999999999997726, 50.00000000000000000 ) ) ;
#1532 = ORIENTED_EDGE ( 'NONE', *, *, #5162, .T. ) ;
#1533 = FILL_AREA_STYLE_COLOUR ( '', #4576 ) ;
#1534 = VECTOR ( 'NONE', #4371, 1000.000000000000000 ) ;
#1535 = ORIENTED_EDGE ( 'NONE', *, *, #1218, .F. ) ;
#1536 = CIRCLE ( 'NONE', #2599, 6.499999999999988454 ) ;
#1537 = DIRECTION ( 'NONE',  ( 0.000000000000000000, -1.000000000000000000, 0.000000000000000000 ) ) ;
#1538 =( LENGTH_UNIT ( ) NAMED_UNIT ( * ) SI_UNIT ( .MILLI., .METRE. ) );
#1539 = ORIENTED_EDGE ( 'NONE', *, *, #3610, .T. ) ;
#1540 = CARTESIAN_POINT ( 'NONE',  ( -2.352990130084610634E-16, 10.39230484541326582, -12.00000000000000000 ) ) ;
#1541 = FILL_AREA_STYLE ('',( #4043 ) ) ;
#1542 = CIRCLE ( 'NONE', #2523, 6.499999999999988454 ) ;
#1543 = ORIENTED_EDGE ( 'NONE', *, *, #4931, .F. ) ;
#1544 = LINE ( 'NONE', #773, #900 ) ;
#1545 = FACE_OUTER_BOUND ( 'NONE', #1662, .T. ) ;
#1546 = FACE_OUTER_BOUND ( 'NONE', #3238, .T. ) ;
#1547 = DIRECTION ( 'NONE',  ( -1.000000000000000000, -0.000000000000000000, -0.000000000000000000 ) ) ;
#1548 = UNCERTAINTY_MEASURE_WITH_UNIT (LENGTH_MEASURE( 1.000000000000000082E-05 ), #1640, 'distance_accuracy_value', 'NONE');
#1549 = SHAPE_DEFINITION_REPRESENTATION ( #4614, #3863 ) ;
#1550 = PRODUCT_RELATED_PRODUCT_CATEGORY ( 'part', '', ( #3432 ) ) ;
#1551 = ORIENTED_EDGE ( 'NONE', *, *, #612, .F. ) ;
#1552 = CARTESIAN_POINT ( 'NONE',  ( -1.144917494144692998E-14, 570.0000000000000000, -24.03599999999999071 ) ) ;
#1553 =( NAMED_UNIT ( * ) PLANE_ANGLE_UNIT ( ) SI_UNIT ( $, .RADIAN. ) );
#1554 = DIRECTION ( 'NONE',  ( -1.000000000000000000, -0.000000000000000000, -0.000000000000000000 ) ) ;
#1555 = FACE_BOUND ( 'NONE', #1013, .T. ) ;
#1556 = CARTESIAN_POINT ( 'NONE',  ( 3.145304002162439438, 9.127642243957637902, -9.190020220263409811 ) ) ;
#1557 = ADVANCED_FACE ( 'NONE', ( #1994 ), #2938, .F. ) ;
#1558 = CARTESIAN_POINT ( 'NONE',  ( -165.0000000000000000, 870.0000000000000000, -5.036000000000040444 ) ) ;
#1559 = CARTESIAN_POINT ( 'NONE',  ( -150.0000000000000284, 10.00000000000000000, 149.9999999999999147 ) ) ;
#1560 =( LENGTH_UNIT ( ) NAMED_UNIT ( * ) SI_UNIT ( .MILLI., .METRE. ) );
#1561 = VERTEX_POINT ( 'NONE', #1096 ) ;
#1562 = FACE_OUTER_BOUND ( 'NONE', #2292, .T. ) ;
#1563 = DIRECTION ( 'NONE',  ( -0.000000000000000000, -1.000000000000000000, -0.000000000000000000 ) ) ;
#1564 = ORIENTED_EDGE ( 'NONE', *, *, #2240, .T. ) ;
#1565 = ORIENTED_EDGE ( 'NONE', *, *, #2151, .F. ) ;
#1566 = ORIENTED_EDGE ( 'NONE', *, *, #328, .F. ) ;
#1567 = LINE ( 'NONE', #4930, #3867 ) ;
#1568 = CYLINDRICAL_SURFACE ( 'NONE', #2592, 20.00000000000001421 ) ;
#1569 = CARTESIAN_POINT ( 'NONE',  ( 6.000000000000000000, 4.379923479639795225, -2.528750000000006271 ) ) ;
#1570 = CARTESIAN_POINT ( 'NONE',  ( 0.000000000000000000, 839.0360000000000582, 0.000000000000000000 ) ) ;
#1571 = APPLICATION_PROTOCOL_DEFINITION ( 'draft international standard', 'automotive_design', 1998, #3109 ) ;
#1572 = EDGE_CURVE ( 'NONE', #4239, #4335, #2381, .T. ) ;
#1573 = ADVANCED_FACE ( 'NONE', ( #719 ), #2415, .T. ) ;
#1574 = LINE ( 'NONE', #4905, #3175 ) ;
#1575 = VERTEX_POINT ( 'NONE', #2768 ) ;
#1576 = CARTESIAN_POINT ( 'NONE',  ( 137.5000000000000000, 870.0000000000000000, -20.00000000000001421 ) ) ;
#1577 = LINE ( 'NONE', #4909, #4491 ) ;
#1578 = CARTESIAN_POINT ( 'NONE',  ( -6.245004513516506329E-15, 610.0000000000000000, 30.00000000000000711 ) ) ;
#1579 = CARTESIAN_POINT ( 'NONE',  ( 1.567730871772294865, 10.05252977580646068, -9.379910571084325355 ) ) ;
#1580 = EDGE_CURVE ( 'NONE', #3738, #4891, #4131, .T. ) ;
#1581 = EDGE_LOOP ( 'NONE', ( #3949, #2582, #4492, #2380 ) ) ;
#1582 = DIRECTION ( 'NONE',  ( 0.000000000000000000, -1.000000000000000000, 0.000000000000000000 ) ) ;
#1583 = CARTESIAN_POINT ( 'NONE',  ( 9.000000000000000000, -2.602085213965210247E-15, -8.419403919045800322 ) ) ;
#1584 = EDGE_LOOP ( 'NONE', ( #1586, #820, #5321, #4418 ) ) ;
#1585 = AXIS2_PLACEMENT_3D ( 'NONE', #2325, #1689, #4966 ) ;
#1586 = ORIENTED_EDGE ( 'NONE', *, *, #3467, .F. ) ;
#1587 = DIRECTION ( 'NONE',  ( 1.000000000000000000, 0.000000000000000000, 0.000000000000000000 ) ) ;
#1588 = AXIS2_PLACEMENT_3D ( 'NONE', #5017, #4274, #3772 ) ;
#1589 = EDGE_LOOP ( 'NONE', ( #4340, #2538, #1674, #2334, #2680, #3027 ) ) ;
#1590 =( NAMED_UNIT ( * ) PLANE_ANGLE_UNIT ( ) SI_UNIT ( $, .RADIAN. ) );
#1591 = VERTEX_POINT ( 'NONE', #3674 ) ;
#1592 = EDGE_CURVE ( 'NONE', #752, #3517, #1340, .T. ) ;
#1593 = AXIS2_PLACEMENT_3D ( 'NONE', #5073, #970, #2548 ) ;
#1594 = EDGE_CURVE ( 'NONE', #1113, #5142, #5246, .T. ) ;
#1595 = ORIENTED_EDGE ( 'NONE', *, *, #2067, .F. ) ;
#1596 = DIRECTION ( 'NONE',  ( 0.000000000000000000, 1.224646799147354933E-16, 1.000000000000000000 ) ) ;
#1597 = CARTESIAN_POINT ( 'NONE',  ( -5.519484922003735861, 7.752549460314756224, -9.137374534098906764 ) ) ;
#1598 = CARTESIAN_POINT ( 'NONE',  ( 121.7157287525372311, 0.000000000000000000, -121.7157287525388369 ) ) ;
#1599 = DIRECTION ( 'NONE',  ( 0.000000000000000000, 0.000000000000000000, 1.000000000000000000 ) ) ;
#1600 = PRESENTATION_LAYER_ASSIGNMENT (  '', '', ( #4912 ) ) ;
#1601 = AXIS2_PLACEMENT_3D ( 'NONE', #3718, #3746, #5371 ) ;
#1602 = LINE ( 'NONE', #3289, #4144 ) ;
#1603 = VERTEX_POINT ( 'NONE', #1961 ) ;
#1604 = CARTESIAN_POINT ( 'NONE',  ( -8.038218111920156501E-16, -10.97743472985186486, -9.686084310752816506 ) ) ;
#1605 = CARTESIAN_POINT ( 'NONE',  ( 25.00000000000000355, 10.00000000000000000, 25.00000000000000000 ) ) ;
#1606 = FACE_OUTER_BOUND ( 'NONE', #1427, .T. ) ;
#1607 = PRODUCT_DEFINITION_CONTEXT ( 'detailed design', #4664, 'design' ) ;
#1608 = PLANE ( 'NONE',  #673 ) ;
#1609 = CIRCLE ( 'NONE', #4230, 14.99999999999998579 ) ;
#1610 = VECTOR ( 'NONE', #5101, 1000.000000000000000 ) ;
#1611 = ORIENTED_EDGE ( 'NONE', *, *, #2928, .T. ) ;
#1612 = DIRECTION ( 'NONE',  ( -1.000000000000000000, 5.551115123125753120E-16, 0.000000000000000000 ) ) ;
#1613 = CARTESIAN_POINT ( 'NONE',  ( -8.250000000000000000, 5.629165124598848990, -8.787392856021023491 ) ) ;
#1614 = ORIENTED_EDGE ( 'NONE', *, *, #1292, .T. ) ;
#1615 = ADVANCED_BREP_SHAPE_REPRESENTATION ( '', ( #3657, #4154 ), #315 ) ;
#1616 = ORIENTED_EDGE ( 'NONE', *, *, #5060, .T. ) ;
#1617 = ADVANCED_FACE ( 'NONE', ( #1492 ), #692, .T. ) ;
#1618 = AXIS2_PLACEMENT_3D ( 'NONE', #4282, #2205, #1460 ) ;
#1619 = AXIS2_PLACEMENT_3D ( 'NONE', #386, #2917, #2497 ) ;
#1620 = SHAPE_REPRESENTATION ( 'support yoke', ( #4154 ), #485 ) ;
#1621 = ORIENTED_EDGE ( 'NONE', *, *, #4781, .T. ) ;
#1622 = DIRECTION ( 'NONE',  ( 0.000000000000000000, 0.000000000000000000, -1.000000000000000000 ) ) ;
#1623 = ORIENTED_EDGE ( 'NONE', *, *, #3900, .F. ) ;
#1624 = CIRCLE ( 'NONE', #2771, 6.000000000000000000 ) ;
#1625 = ORIENTED_EDGE ( 'NONE', *, *, #5027, .F. ) ;
#1626 =( LENGTH_UNIT ( ) NAMED_UNIT ( * ) SI_UNIT ( .MILLI., .METRE. ) );
#1627 = EDGE_LOOP ( 'NONE', ( #3668, #4592, #625, #2747 ) ) ;
#1628 = VECTOR ( 'NONE', #5025, 1000.000000000000000 ) ;
#1629 = VECTOR ( 'NONE', #364, 1000.000000000000000 ) ;
#1630 = ORIENTED_EDGE ( 'NONE', *, *, #5039, .T. ) ;
#1631 = DIRECTION ( 'NONE',  ( 0.000000000000000000, -1.000000000000000000, 0.000000000000000000 ) ) ;
#1632 = EDGE_CURVE ( 'NONE', #2355, #3602, #3201, .T. ) ;
#1633 = CARTESIAN_POINT ( 'NONE',  ( -3.070858717647508396, 9.166611990351359651, -9.141698485139983177 ) ) ;
#1634 = SHAPE_REPRESENTATION ( 'hex flange nut gradea_iso_ISO - 4161 - M12 - N', ( #4154 ), #315 ) ;
#1635 = FACE_OUTER_BOUND ( 'NONE', #1658, .T. ) ;
#1636 = CARTESIAN_POINT ( 'NONE',  ( -9.000000000000000000, -0.9015406389697722123, 1.312336379612662396E-15 ) ) ;
#1637 = CIRCLE ( 'NONE', #2333, 5.035999999999999588 ) ;
#1638 = APPLICATION_PROTOCOL_DEFINITION ( 'draft international standard', 'automotive_design', 1998, #109 ) ;
#1639 = CIRCLE ( 'NONE', #2609, 6.499999999999988454 ) ;
#1640 =( LENGTH_UNIT ( ) NAMED_UNIT ( * ) SI_UNIT ( .MILLI., .METRE. ) );
#1641 = VERTEX_POINT ( 'NONE', #4054 ) ;
#1642 = CARTESIAN_POINT ( 'NONE',  ( 8.327614167581914066E-17, -10.39230484541327115, -9.106324069981644342 ) ) ;
#1643 = SURFACE_STYLE_USAGE ( .BOTH. , #35 ) ;
#1644 = FACE_OUTER_BOUND ( 'NONE', #2459, .T. ) ;
#1645 = CARTESIAN_POINT ( 'NONE',  ( 150.0000000000000000, 810.0000000000000000, 25.00000000000000000 ) ) ;
#1646 = CARTESIAN_POINT ( 'NONE',  ( 121.7157287525372311, 0.000000000000000000, -106.7157287525388369 ) ) ;
#1647 = FACE_OUTER_BOUND ( 'NONE', #3306, .T. ) ;
#1648 = EDGE_LOOP ( 'NONE', ( #1052, #3103 ) ) ;
#1649 = EDGE_LOOP ( 'NONE', ( #2000, #1142 ) ) ;
#1650 = EDGE_LOOP ( 'NONE', ( #3412, #1621, #4704, #1985, #1506 ) ) ;
#1651 = EDGE_CURVE ( 'NONE', #3303, #3154, #3622, .T. ) ;
#1652 = ORIENTED_EDGE ( 'NONE', *, *, #194, .F. ) ;
#1653 = ADVANCED_FACE ( 'NONE', ( #4851, #337 ), #1125, .F. ) ;
#1654 = LINE ( 'NONE', #730, #128 ) ;
#1655 = VERTEX_POINT ( 'NONE', #5329 ) ;
#1656 = ORIENTED_EDGE ( 'NONE', *, *, #2518, .T. ) ;
#1657 = ORIENTED_EDGE ( 'NONE', *, *, #5072, .T. ) ;
#1658 = EDGE_LOOP ( 'NONE', ( #3325, #1595, #1614, #732 ) ) ;
#1659 = FACE_OUTER_BOUND ( 'NONE', #534, .T. ) ;
#1660 = CARTESIAN_POINT ( 'NONE',  ( 6.134460314789567548, -6.850572531336434068, -8.512883888440004654 ) ) ;
#1661 = CONTEXT_DEPENDENT_SHAPE_REPRESENTATION ( #3074, #1789 ) ;
#1662 = EDGE_LOOP ( 'NONE', ( #4437, #810, #4037, #1804 ) ) ;
#1663 = PLANE ( 'NONE',  #1325 ) ;
#1664 = DIRECTION ( 'NONE',  ( -1.000000000000000000, -0.000000000000000000, -0.000000000000000000 ) ) ;
#1665 =( GEOMETRIC_REPRESENTATION_CONTEXT ( 3 ) GLOBAL_UNCERTAINTY_ASSIGNED_CONTEXT ( ( #1122 ) ) GLOBAL_UNIT_ASSIGNED_CONTEXT ( ( #3066, #4242, #933 ) ) REPRESENTATION_CONTEXT ( 'NONE', 'WORKASPACE' ) );
#1666 = CARTESIAN_POINT ( 'NONE',  ( 0.000000000000000000, 10.00000000000000000, 0.000000000000000000 ) ) ;
#1667 = EDGE_CURVE ( 'NONE', #5291, #1919, #2890, .T. ) ;
#1668 = CARTESIAN_POINT ( 'NONE',  ( 8.250000000000000000, -5.629165124598856984, -8.787392856021023491 ) ) ;
#1669 = EDGE_CURVE ( 'NONE', #2957, #3489, #1574, .T. ) ;
#1670 = EDGE_CURVE ( 'NONE', #3556, #1913, #1602, .T. ) ;
#1671 = ORIENTED_EDGE ( 'NONE', *, *, #1572, .T. ) ;
#1672 = CARTESIAN_POINT ( 'NONE',  ( 3.712196824332475220, 8.249067009600011602, -8.964894084809515107 ) ) ;
#1673 = FACE_OUTER_BOUND ( 'NONE', #3685, .T. ) ;
#1674 = ORIENTED_EDGE ( 'NONE', *, *, #1177, .T. ) ;
#1675 = ORIENTED_EDGE ( 'NONE', *, *, #814, .T. ) ;
#1676 = CARTESIAN_POINT ( 'NONE',  ( -164.0360000000000014, 870.0000000000000000, 0.000000000000000000 ) ) ;
#1677 = ORIENTED_EDGE ( 'NONE', *, *, #4751, .T. ) ;
#1678 = ORIENTED_EDGE ( 'NONE', *, *, #3048, .T. ) ;
#1679 = CIRCLE ( 'NONE', #4634, 9.000000000000000000 ) ;
#1680 = ORIENTED_EDGE ( 'NONE', *, *, #3610, .F. ) ;
#1681 = CARTESIAN_POINT ( 'NONE',  ( 165.0000000000000000, 870.0000000000000000, 0.000000000000000000 ) ) ;
#1682 = DIRECTION ( 'NONE',  ( 0.000000000000000000, 1.000000000000000000, 0.000000000000000000 ) ) ;
#1683 = CARTESIAN_POINT ( 'NONE',  ( 6.499999999999981348, 35.00000000000000000, 30.00000000000000711 ) ) ;
#1684 = ITEM_DEFINED_TRANSFORMATION ( 'NONE', 'NONE', #400,  #4154 ) ;
#1685 = AXIS2_PLACEMENT_3D ( 'NONE', #890, #55, #4643 ) ;
#1686 = EDGE_CURVE ( 'NONE', #2061, #2556, #4819, .T. ) ;
#1687 = DIRECTION ( 'NONE',  ( -1.000000000000000000, -0.000000000000000000, -0.000000000000000000 ) ) ;
#1688 = AXIS2_PLACEMENT_3D ( 'NONE', #4682, #1828, #4287 ) ;
#1689 = DIRECTION ( 'NONE',  ( -1.000000000000000000, -0.000000000000000000, -0.000000000000000000 ) ) ;
#1690 = FACE_OUTER_BOUND ( 'NONE', #2461, .T. ) ;
#1691 = CARTESIAN_POINT ( 'NONE',  ( -4.500000000000003553, 7.794228634059947147, 0.000000000000000000 ) ) ;
#1692 = CARTESIAN_POINT ( 'NONE',  ( 0.000000000000000000, -10.39230484541327293, -8.935996291721338025 ) ) ;
#1693 = SURFACE_STYLE_FILL_AREA ( #3663 ) ;
#1694 = CIRCLE ( 'NONE', #3014, 6.000000000000000000 ) ;
#1695 = PLANE ( 'NONE',  #3064 ) ;
#1696 = DIRECTION ( 'NONE',  ( -0.000000000000000000, -0.000000000000000000, 1.000000000000000000 ) ) ;
#1697 = PLANE ( 'NONE',  #2774 ) ;
#1698 = CIRCLE ( 'NONE', #1948, 14.99999999999998579 ) ;
#1699 = ADVANCED_FACE ( 'NONE', ( #3230 ), #4880, .F. ) ;
#1700 = COLOUR_RGB ( '',0.8941176470588234615, 0.8941176470588234615, 0.8941176470588234615 ) ;
#1701 = ORIENTED_EDGE ( 'NONE', *, *, #3430, .F. ) ;
#1702 = VERTEX_POINT ( 'NONE', #1236 ) ;
#1703 = EDGE_LOOP ( 'NONE', ( #4334, #4590 ) ) ;
#1704 = CLOSED_SHELL ( 'NONE', ( #4182, #4266, #848, #2419, #4143, #3046, #3376, #3139, #5154, #3778, #3323, #3865, #1313, #4477, #5357, #1813, #1573, #2678, #1085, #3540, #4827, #2531, #212, #1733, #471 ) ) ;
#1705 = EDGE_CURVE ( 'NONE', #1732, #2368, #3364, .T. ) ;
#1706 = ADVANCED_FACE ( 'NONE', ( #4436 ), #1057, .F. ) ;
#1707 = CIRCLE ( 'NONE', #1423, 6.000000000000005329 ) ;
#1708 = COLOUR_RGB ( '',1.000000000000000000, 0.9490196078431372140, 0.9098039215686274384 ) ;
#1709 = DIRECTION ( 'NONE',  ( 0.000000000000000000, -0.8660254037844391517, -0.4999999999999991118 ) ) ;
#1710 = CIRCLE ( 'NONE', #4740, 9.000000000000000000 ) ;
#1711 = AXIS2_PLACEMENT_3D ( 'NONE', #5126, #948, #2182 ) ;
#1712 = ORIENTED_EDGE ( 'NONE', *, *, #3751, .T. ) ;
#1713 = DIRECTION ( 'NONE',  ( 1.000000000000000000, 0.000000000000000000, 0.000000000000000000 ) ) ;
#1714 = CARTESIAN_POINT ( 'NONE',  ( 0.05527946870651088973, 11.01006727514131356, -9.698012095152311218 ) ) ;
#1715 = CYLINDRICAL_SURFACE ( 'NONE', #4005, 9.000000000000000000 ) ;
#1716 = CONTEXT_DEPENDENT_SHAPE_REPRESENTATION ( #2805, #5243 ) ;
#1717 = AXIS2_PLACEMENT_3D ( 'NONE', #3591, #1442, #2693 ) ;
#1718 = EDGE_CURVE ( 'NONE', #4147, #4026, #4642, .T. ) ;
#1719 = DIRECTION ( 'NONE',  ( 6.938893903907228378E-17, 0.000000000000000000, -1.000000000000000000 ) ) ;
#1720 = LINE ( 'NONE', #5048, #4511 ) ;
#1721 = DIRECTION ( 'NONE',  ( 0.000000000000000000, 0.000000000000000000, 1.000000000000000000 ) ) ;
#1722 = EDGE_CURVE ( 'NONE', #754, #3611, #1084, .T. ) ;
#1723 = AXIS2_PLACEMENT_3D ( 'NONE', #2570, #2937, #1305 ) ;
#1724 = CARTESIAN_POINT ( 'NONE',  ( -1.453914506656639238, 9.552886913616349673, -0.5405968996908959712 ) ) ;
#1725 = ORIENTED_EDGE ( 'NONE', *, *, #3298, .T. ) ;
#1726 = CARTESIAN_POINT ( 'NONE',  ( -9.000000000001600498, 3.788414693531317656, -9.200428974772291824 ) ) ;
#1727 = AXIS2_PLACEMENT_3D ( 'NONE', #2764, #333, #4108 ) ;
#1728 = EDGE_LOOP ( 'NONE', ( #417, #3099 ) ) ;
#1729 = DIRECTION ( 'NONE',  ( 0.000000000000000000, 0.000000000000000000, -1.000000000000000000 ) ) ;
#1730 = CARTESIAN_POINT ( 'NONE',  ( 7.828285197793313444, 5.872642279174128177, -8.684787165848931068 ) ) ;
#1731 = CARTESIAN_POINT ( 'NONE',  ( 25.00000000000000355, 60.00000000000000711, 25.00000000000000000 ) ) ;
#1732 = VERTEX_POINT ( 'NONE', #3869 ) ;
#1733 = ADVANCED_FACE ( 'NONE', ( #3490 ), #2567, .F. ) ;
#1734 = CARTESIAN_POINT ( 'NONE',  ( 6.000000000000000000, -5.839897972853064445, 4.770489558936219510E-15 ) ) ;
#1735 = EDGE_LOOP ( 'NONE', ( #2336, #2444, #4389, #3297 ) ) ;
#1736 = EDGE_CURVE ( 'NONE', #2365, #1561, #3051, .T. ) ;
#1737 = ORIENTED_EDGE ( 'NONE', *, *, #3481, .F. ) ;
#1738 = DIRECTION ( 'NONE',  ( 0.000000000000000000, -0.5000000000000008882, -0.8660254037844380415 ) ) ;
#1739 = CARTESIAN_POINT ( 'NONE',  ( -121.7157287525381122, -20.00000000000000000, 121.7157287525380127 ) ) ;
#1740 = CARTESIAN_POINT ( 'NONE',  ( 0.000000000000000000, 0.000000000000000000, 0.000000000000000000 ) ) ;
#1741 = CARTESIAN_POINT ( 'NONE',  ( 7.727639453308645656, -5.930750126846072945, -9.220334578152900917 ) ) ;
#1742 = CARTESIAN_POINT ( 'NONE',  ( -9.000000000000000000, 3.091092034686353518, -0.4369508170668109925 ) ) ;
#1743 = ORIENTED_EDGE ( 'NONE', *, *, #1341, .F. ) ;
#1744 = DIRECTION ( 'NONE',  ( 1.000000000000000000, -0.000000000000000000, -0.000000000000000000 ) ) ;
#1745 =( NAMED_UNIT ( * ) SI_UNIT ( $, .STERADIAN. ) SOLID_ANGLE_UNIT ( ) );
#1746 = DIRECTION ( 'NONE',  ( 1.000000000000000000, 0.000000000000000000, 0.000000000000000000 ) ) ;
#1747 = ADVANCED_FACE ( 'NONE', ( #2671 ), #5120, .T. ) ;
#1748 = PLANE ( 'NONE',  #2875 ) ;
#1749 = PRODUCT ( 'Vertical Telescoping Support Column', 'Vertical Telescoping Support Column', '', ( #4877 ) ) ;
#1750=STYLED_ITEM('',(#5440),#104);
#1751 = ORIENTED_EDGE ( 'NONE', *, *, #5316, .F. ) ;
#1752 = DIRECTION ( 'NONE',  ( 1.000000000000000000, 0.000000000000000000, 0.000000000000000000 ) ) ;
#1753 = CARTESIAN_POINT ( 'NONE',  ( 1.215778977584813125, 9.690374525429584551, -8.707326526324868254 ) ) ;
#1754 = CARTESIAN_POINT ( 'NONE',  ( 9.000000000000001776, 3.091092034686357071, -0.4369508170668111591 ) ) ;
#1755 = EDGE_CURVE ( 'NONE', #1094, #1655, #2696, .T. ) ;
#1756 = PLANE ( 'NONE',  #3881 ) ;
#1757 = ORIENTED_EDGE ( 'NONE', *, *, #206, .T. ) ;
#1758 = CARTESIAN_POINT ( 'NONE',  ( -25.00000000000000000, 610.0000000000000000, 24.99999999999999645 ) ) ;
#1759 = LINE ( 'NONE', #4692, #3954 ) ;
#1760 = PLANE ( 'NONE',  #3565 ) ;
#1761 = CONTEXT_DEPENDENT_SHAPE_REPRESENTATION ( #1918, #4450 ) ;
#1762 = EDGE_CURVE ( 'NONE', #3352, #539, #83, .T. ) ;
#1763 = ADVANCED_FACE ( 'NONE', ( #3843 ), #2492, .F. ) ;
#1764 = DIRECTION ( 'NONE',  ( 0.000000000000000000, 0.000000000000000000, -1.000000000000000000 ) ) ;
#1765 = CARTESIAN_POINT ( 'NONE',  ( -1.676835913137321903E-15, 35.00000000000000000, 25.00000000000000000 ) ) ;
#1766 = FACE_BOUND ( 'NONE', #4681, .T. ) ;
#1767 = CARTESIAN_POINT ( 'NONE',  ( 12.00000000000000000, 8.082668874372532992E-16, 6.600000000000001421 ) ) ;
#1768 = DIRECTION ( 'NONE',  ( 9.251858538542972814E-17, 0.000000000000000000, -1.000000000000000000 ) ) ;
#1769 = AXIS2_PLACEMENT_3D ( 'NONE', #3034, #4675, #947 ) ;
#1770 = ORIENTED_EDGE ( 'NONE', *, *, #1109, .T. ) ;
#1771 = VECTOR ( 'NONE', #5024, 1000.000000000000000 ) ;
#1772 = DIRECTION ( 'NONE',  ( 0.000000000000000000, -1.000000000000000000, 0.000000000000000000 ) ) ;
#1773 = CARTESIAN_POINT ( 'NONE',  ( 139.9999999999999716, 885.0000000000000000, 25.00000000000000000 ) ) ;
#1774 = PLANE ( 'NONE',  #4397 ) ;
#1775 = UNCERTAINTY_MEASURE_WITH_UNIT (LENGTH_MEASURE( 1.000000000000000082E-05 ), #3570, 'distance_accuracy_value', 'NONE');
#1776 = FACE_OUTER_BOUND ( 'NONE', #2546, .T. ) ;
#1777 = VECTOR ( 'NONE', #5215, 1000.000000000000000 ) ;
#1778 = LINE ( 'NONE', #5084, #562 ) ;
#1779 = ORIENTED_EDGE ( 'NONE', *, *, #4990, .F. ) ;
#1780 = VECTOR ( 'NONE', #1825, 1000.000000000000000 ) ;
#1781 = AXIS2_PLACEMENT_3D ( 'NONE', #3811, #934, #3785 ) ;
#1782 =( GEOMETRIC_REPRESENTATION_CONTEXT ( 3 ) GLOBAL_UNCERTAINTY_ASSIGNED_CONTEXT ( ( #301 ) ) GLOBAL_UNIT_ASSIGNED_CONTEXT ( ( #2011, #1590, #4806 ) ) REPRESENTATION_CONTEXT ( 'NONE', 'WORKASPACE' ) );
#1783 = ORIENTED_EDGE ( 'NONE', *, *, #535, .F. ) ;
#1784 = DIRECTION ( 'NONE',  ( -0.000000000000000000, -1.000000000000000000, -0.000000000000000000 ) ) ;
#1785 = AXIS2_PLACEMENT_3D ( 'NONE', #2894, #3616, #1181 ) ;
#1786 = LINE ( 'NONE', #2093, #5353 ) ;
#1787 =( GEOMETRIC_REPRESENTATION_CONTEXT ( 3 ) GLOBAL_UNCERTAINTY_ASSIGNED_CONTEXT ( ( #4190 ) ) GLOBAL_UNIT_ASSIGNED_CONTEXT ( ( #3858, #4097, #4997 ) ) REPRESENTATION_CONTEXT ( 'NONE', 'WORKASPACE' ) );
#1788 = DIRECTION ( 'NONE',  ( 1.000000000000000000, 0.000000000000000000, 0.000000000000000000 ) ) ;
#1789 = PRODUCT_DEFINITION_SHAPE ( 'NONE', 'NONE',  #5394 ) ;
#1790 = AXIS2_PLACEMENT_3D ( 'NONE', #1494, #3169, #5248 ) ;
#1791 = EDGE_CURVE ( 'NONE', #2061, #1418, #3073, .T. ) ;
#1792 = EDGE_CURVE ( 'NONE', #601, #3466, #832, .T. ) ;
#1793 = CARTESIAN_POINT ( 'NONE',  ( -9.000000000000000000, 5.196152422706629359, -1.199999999999997291 ) ) ;
#1794 = VERTEX_POINT ( 'NONE', #3028 ) ;
#1795 = CARTESIAN_POINT ( 'NONE',  ( -164.0360000000000014, 870.0000000000000000, 0.000000000000000000 ) ) ;
#1796 = LINE ( 'NONE', #520, #3389 ) ;
#1797 = CARTESIAN_POINT ( 'NONE',  ( -9.000000000000000000, 1.732050807568874085, -8.505011083697295859 ) ) ;
#1798 = ORIENTED_EDGE ( 'NONE', *, *, #2100, .T. ) ;
#1799 = FACE_OUTER_BOUND ( 'NONE', #1581, .T. ) ;
#1800 = DIRECTION ( 'NONE',  ( 1.000000000000000000, 0.000000000000000000, 0.000000000000000000 ) ) ;
#1801 = ORIENTED_EDGE ( 'NONE', *, *, #4432, .T. ) ;
#1802 = CONICAL_SURFACE ( 'NONE', #5299, 9.000000000000001776, 0.8594454914424796144 ) ;
#1803 = FACE_OUTER_BOUND ( 'NONE', #668, .T. ) ;
#1804 = ORIENTED_EDGE ( 'NONE', *, *, #4657, .F. ) ;
#1805 = DIRECTION ( 'NONE',  ( -1.000000000000000000, -0.000000000000000000, 0.000000000000000000 ) ) ;
#1806 = CARTESIAN_POINT ( 'NONE',  ( 121.7157287525384533, -20.00000000000000000, 136.7157287525376717 ) ) ;
#1807 = DIRECTION ( 'NONE',  ( -0.000000000000000000, -1.000000000000000000, -0.000000000000000000 ) ) ;
#1808 = DIRECTION ( 'NONE',  ( 0.000000000000000000, 0.000000000000000000, 1.000000000000000000 ) ) ;
#1809 = AXIS2_PLACEMENT_3D ( 'NONE', #3644, #4934, #1599 ) ;
#1810 = PRODUCT_DEFINITION_SHAPE ( 'NONE', 'NONE',  #4517 ) ;
#1811 = CARTESIAN_POINT ( 'NONE',  ( -6.000000000000000000, 7.347880794884119736E-16, 0.000000000000000000 ) ) ;
#1812 = MANIFOLD_SOLID_BREP ( 'LPattern1', #5093 ) ;
#1813 = ADVANCED_FACE ( 'NONE', ( #4863 ), #1320, .T. ) ;
#1814 = PRESENTATION_STYLE_ASSIGNMENT (( #152 ) ) ;
#1815 = ADVANCED_FACE ( 'NONE', ( #4330 ), #236, .F. ) ;
#1816 = EDGE_LOOP ( 'NONE', ( #242, #75 ) ) ;
#1817 = CARTESIAN_POINT ( 'NONE',  ( 137.5000000000000000, 870.0000000000000000, 20.00000000000001421 ) ) ;
#1818 = LINE ( 'NONE', #5091, #2435 ) ;
#1819 = MANIFOLD_SOLID_BREP ( 'Hex', #2750 ) ;
#1820 = EDGE_LOOP ( 'NONE', ( #1346, #3792, #1335, #3477, #3130 ) ) ;
#1821 = DIRECTION ( 'NONE',  ( 1.000000000000000000, 0.000000000000000000, 0.000000000000000000 ) ) ;
#1822 = CARTESIAN_POINT ( 'NONE',  ( -150.0000000000000000, 870.0000000000000000, 5.999999999999950262 ) ) ;
#1823 = DIRECTION ( 'NONE',  ( -1.000000000000000000, 0.000000000000000000, 0.000000000000000000 ) ) ;
#1824 = ORIENTED_EDGE ( 'NONE', *, *, #4857, .F. ) ;
#1825 = DIRECTION ( 'NONE',  ( -1.000000000000000000, 0.000000000000000000, -0.000000000000000000 ) ) ;
#1826 = DIRECTION ( 'NONE',  ( 0.000000000000000000, 1.000000000000000000, 0.000000000000000000 ) ) ;
#1827 = EDGE_CURVE ( 'NONE', #701, #3600, #3182, .T. ) ;
#1828 = DIRECTION ( 'NONE',  ( 0.000000000000000000, 1.000000000000000000, 0.000000000000000000 ) ) ;
#1829 = DIRECTION ( 'NONE',  ( 0.8191520442889915765, 0.000000000000000000, 0.5735764363510464925 ) ) ;
#1830 = FACE_OUTER_BOUND ( 'NONE', #3347, .T. ) ;
#1831 = LINE ( 'NONE', #3148, #234 ) ;
#1832 = EDGE_CURVE ( 'NONE', #4959, #1094, #1967, .T. ) ;
#1833 = ADVANCED_FACE ( 'NONE', ( #2278 ), #1505, .T. ) ;
#1834 = DIRECTION ( 'NONE',  ( 0.7071067811865577868, 0.000000000000000000, -0.7071067811865373587 ) ) ;
#1835 = CARTESIAN_POINT ( 'NONE',  ( 1.500000000000000666, 9.526279441628828337, -8.667800885990208926 ) ) ;
#1836 = VECTOR ( 'NONE', #93, 1000.000000000000000 ) ;
#1837 = ORIENTED_EDGE ( 'NONE', *, *, #4196, .F. ) ;
#1838 = CARTESIAN_POINT ( 'NONE',  ( -9.477403599784569366, -1.836490901034005807, -9.189746347754448763 ) ) ;
#1839 = CARTESIAN_POINT ( 'NONE',  ( -25.00000000000000000, 810.0000000000000000, 24.99999999999999645 ) ) ;
#1840 = DIRECTION ( 'NONE',  ( -0.000000000000000000, -0.000000000000000000, 1.000000000000000000 ) ) ;
#1841 = EDGE_LOOP ( 'NONE', ( #1033, #2082 ) ) ;
#1842 = CARTESIAN_POINT ( 'NONE',  ( -121.7157287525392917, -20.00000000000000000, -121.7157287525368332 ) ) ;
#1843 = LINE ( 'NONE', #973, #3737 ) ;
#1844 = CARTESIAN_POINT ( 'NONE',  ( 74.99999999999998579, 557.4999999999997726, 50.00000000000002132 ) ) ;
#1845 = DIRECTION ( 'NONE',  ( 0.000000000000000000, 0.000000000000000000, -1.000000000000000000 ) ) ;
#1846 = ORIENTED_EDGE ( 'NONE', *, *, #2792, .F. ) ;
#1847 = ORIENTED_EDGE ( 'NONE', *, *, #473, .F. ) ;
#1848 = DIRECTION ( 'NONE',  ( -1.000000000000000000, 0.000000000000000000, 1.387778780781445676E-16 ) ) ;
#1849 = CARTESIAN_POINT ( 'NONE',  ( 0.000000000000000000, 330.0000000000000000, 25.00000000000000000 ) ) ;
#1850 = CARTESIAN_POINT ( 'NONE',  ( -6.499999999999988454, 450.0000000000000000, -25.00000000000000000 ) ) ;
#1851 = AXIS2_PLACEMENT_3D ( 'NONE', #61, #32, #1719 ) ;
#1852 = EDGE_CURVE ( 'NONE', #529, #4871, #2843, .T. ) ;
#1853 = CARTESIAN_POINT ( 'NONE',  ( 25.00000000000000355, 60.00000000000000711, 25.00000000000000000 ) ) ;
#1854 = LINE ( 'NONE', #2302, #1026 ) ;
#1855 =( GEOMETRIC_REPRESENTATION_CONTEXT ( 3 ) GLOBAL_UNCERTAINTY_ASSIGNED_CONTEXT ( ( #1548 ) ) GLOBAL_UNIT_ASSIGNED_CONTEXT ( ( #1640, #4964, #942 ) ) REPRESENTATION_CONTEXT ( 'NONE', 'WORKASPACE' ) );
#1856 = VERTEX_POINT ( 'NONE', #1477 ) ;
#1857 = ORIENTED_EDGE ( 'NONE', *, *, #4656, .T. ) ;
#1858 = AXIS2_PLACEMENT_3D ( 'NONE', #97, #5041, #3433 ) ;
#1859 = ORIENTED_EDGE ( 'NONE', *, *, #4409, .T. ) ;
#1860 = DIRECTION ( 'NONE',  ( 0.000000000000000000, -1.000000000000000000, 0.000000000000000000 ) ) ;
#1861 = VERTEX_POINT ( 'NONE', #3131 ) ;
#1862 = CARTESIAN_POINT ( 'NONE',  ( -74.99999999999998579, 557.4999999999997726, 29.99999999999999289 ) ) ;
#1863 = PRODUCT_DEFINITION_FORMATION_WITH_SPECIFIED_SOURCE ( 'ANY', '', #2139, .NOT_KNOWN. ) ;
#1864 = DIRECTION ( 'NONE',  ( 1.000000000000000000, 0.000000000000000000, 0.000000000000000000 ) ) ;
#1865 = CIRCLE ( 'NONE', #1344, 12.38940648156203927 ) ;
#1866 = AXIS2_PLACEMENT_3D ( 'NONE', #3854, #542, #3138 ) ;
#1867 = ORIENTED_EDGE ( 'NONE', *, *, #2240, .F. ) ;
#1868 = ORIENTED_EDGE ( 'NONE', *, *, #1762, .F. ) ;
#1869 = CARTESIAN_POINT ( 'NONE',  ( -2.352990130084610634E-16, 10.39230484541326582, -8.935996291721336249 ) ) ;
#1870 = FACE_BOUND ( 'NONE', #1649, .T. ) ;
#1871 = CARTESIAN_POINT ( 'NONE',  ( 0.000000000000000000, 2.919948986426538440, 5.057499999999994778 ) ) ;
#1872 = CARTESIAN_POINT ( 'NONE',  ( 6.499999999999981348, 35.00000000000000000, -30.00000000000000711 ) ) ;
#1873 = PRESENTATION_STYLE_ASSIGNMENT (( #1434 ) ) ;
#1874 = ADVANCED_FACE ( 'NONE', ( #4837 ), #4729, .T. ) ;
#1875 = VECTOR ( 'NONE', #4339, 1000.000000000000000 ) ;
#1876 =( GEOMETRIC_REPRESENTATION_CONTEXT ( 3 ) GLOBAL_UNCERTAINTY_ASSIGNED_CONTEXT ( ( #4935 ) ) GLOBAL_UNIT_ASSIGNED_CONTEXT ( ( #4853, #2021, #4941 ) ) REPRESENTATION_CONTEXT ( 'NONE', 'WORKASPACE' ) );
#1877 = ORIENTED_EDGE ( 'NONE', *, *, #842, .F. ) ;
#1878 = EDGE_CURVE ( 'NONE', #1195, #353, #49, .T. ) ;
#1879 = CARTESIAN_POINT ( 'NONE',  ( 8.999999999999998224, -3.516072269208508683, -0.5641419778896282766 ) ) ;
#1880 = EDGE_LOOP ( 'NONE', ( #925, #1095, #4640, #392 ) ) ;
#1881 = FILL_AREA_STYLE ('',( #4057 ) ) ;
#1882 = LINE ( 'NONE', #2739, #4659 ) ;
#1883 = CARTESIAN_POINT ( 'NONE',  ( -6.499999999999984901, 35.00000000000000000, -25.00000000000000000 ) ) ;
#1884 = LINE ( 'NONE', #5250, #3116 ) ;
#1885 = CONICAL_SURFACE ( 'NONE', #3031, 5.999999999999996447, 0.7853981633974074228 ) ;
#1886 = CARTESIAN_POINT ( 'NONE',  ( 9.000000000000000000, 1.854613033839518588, -9.019235192255276701 ) ) ;
#1887 = CARTESIAN_POINT ( 'NONE',  ( -25.00000000000000000, 60.00000000000000711, 25.00000000000000000 ) ) ;
#1888 = VERTEX_POINT ( 'NONE', #2723 ) ;
#1889 = ADVANCED_FACE ( 'NONE', ( #2751, #4406 ), #4374, .F. ) ;
#1890 = VECTOR ( 'NONE', #516, 1000.000000000000000 ) ;
#1891 = ORIENTED_EDGE ( 'NONE', *, *, #284, .F. ) ;
#1892 = CARTESIAN_POINT ( 'NONE',  ( -9.473745496805531019, -0.9193675319299582371, -9.138786188337409300 ) ) ;
#1893 = ORIENTED_EDGE ( 'NONE', *, *, #4322, .F. ) ;
#1894 = DIRECTION ( 'NONE',  ( -1.000000000000000000, -0.000000000000000000, -0.000000000000000000 ) ) ;
#1895 = CARTESIAN_POINT ( 'NONE',  ( 0.000000000000000000, 570.0000000000000000, 30.00000000000000711 ) ) ;
#1896 = EDGE_CURVE ( 'NONE', #3246, #2365, #2308, .T. ) ;
#1897 = ADVANCED_FACE ( 'NONE', ( #260 ), #2009, .F. ) ;
#1898 = EDGE_CURVE ( 'NONE', #1919, #5042, #1694, .T. ) ;
#1899 = ORIENTED_EDGE ( 'NONE', *, *, #1669, .F. ) ;
#1900 = CARTESIAN_POINT ( 'NONE',  ( 6.000000000000000888, 0.000000000000000000, -12.00000000000000000 ) ) ;
#1901 = LINE ( 'NONE', #2406, #2958 ) ;
#1902 = DIRECTION ( 'NONE',  ( 0.000000000000000000, 0.000000000000000000, 1.000000000000000000 ) ) ;
#1903 = DIRECTION ( 'NONE',  ( 1.000000000000000000, 0.000000000000000000, 0.000000000000000000 ) ) ;
#1904 = SURFACE_STYLE_FILL_AREA ( #215 ) ;
#1905 = EDGE_CURVE ( 'NONE', #4719, #2454, #3093, .T. ) ;
#1906 = CARTESIAN_POINT ( 'NONE',  ( 0.000000000000000000, 390.0000000000000000, -25.00000000000000000 ) ) ;
#1907 = DIRECTION ( 'NONE',  ( 0.000000000000000000, -0.4999999999999991118, 0.8660254037844390407 ) ) ;
#1908 = FACE_OUTER_BOUND ( 'NONE', #637, .T. ) ;
#1909 = CYLINDRICAL_SURFACE ( 'NONE', #488, 15.00000000000000000 ) ;
#1910 = CARTESIAN_POINT ( 'NONE',  ( 74.99999999999998579, 557.4999999999997726, 30.00000000000002487 ) ) ;
#1911 = DIRECTION ( 'NONE',  ( 0.000000000000000000, 0.000000000000000000, 1.000000000000000000 ) ) ;
#1912 = CARTESIAN_POINT ( 'NONE',  ( 24.99999999999999645, 60.00000000000000711, -25.00000000000000000 ) ) ;
#1913 = VERTEX_POINT ( 'NONE', #4069 ) ;
#1914 = ORIENTED_EDGE ( 'NONE', *, *, #842, .T. ) ;
#1915 = EDGE_CURVE ( 'NONE', #2252, #5301, #2306, .T. ) ;
#1916 = AXIS2_PLACEMENT_3D ( 'NONE', #3041, #955, #4289 ) ;
#1917 = VECTOR ( 'NONE', #548, 999.9999999999998863 ) ;
#1918 =( REPRESENTATION_RELATIONSHIP ('NONE','NONE', #4791, #1634 ) REPRESENTATION_RELATIONSHIP_WITH_TRANSFORMATION ( #1684 )SHAPE_REPRESENTATION_RELATIONSHIP( ) );
#1919 = VERTEX_POINT ( 'NONE', #4924 ) ;
#1920 = DIRECTION ( 'NONE',  ( 0.000000000000000000, -0.000000000000000000, -1.000000000000000000 ) ) ;
#1921 = ORIENTED_EDGE ( 'NONE', *, *, #1667, .T. ) ;
#1922 = ORIENTED_EDGE ( 'NONE', *, *, #876, .T. ) ;
#1923 = CARTESIAN_POINT ( 'NONE',  ( -1.144917494144692998E-14, 570.0000000000000000, 30.00000000000001066 ) ) ;
#1924 = DIRECTION ( 'NONE',  ( 1.000000000000000000, 0.000000000000000000, 2.081668171172168513E-16 ) ) ;
#1925 = CARTESIAN_POINT ( 'NONE',  ( -139.9999999999999716, 870.0000000000000000, 0.000000000000000000 ) ) ;
#1926 = ADVANCED_FACE ( 'NONE', ( #5318 ), #2399, .F. ) ;
#1927 = CARTESIAN_POINT ( 'NONE',  ( -25.00000000000000000, 60.00000000000000711, 25.00000000000000000 ) ) ;
#1928 = ADVANCED_FACE ( 'NONE', ( #793 ), #818, .F. ) ;
#1929 = ORIENTED_EDGE ( 'NONE', *, *, #1992, .T. ) ;
#1930 = ORIENTED_EDGE ( 'NONE', *, *, #5007, .T. ) ;
#1931 = DIRECTION ( 'NONE',  ( 1.000000000000000000, 0.000000000000000000, 0.000000000000000000 ) ) ;
#1932 = CARTESIAN_POINT ( 'NONE',  ( 6.499999999999988454, 570.0000000000000000, 25.00000000000000000 ) ) ;
#1933 = CARTESIAN_POINT ( 'NONE',  ( 6.499999999999988454, 390.0000000000000000, 25.00000000000000000 ) ) ;
#1934 = DIRECTION ( 'NONE',  ( -1.000000000000000000, -0.000000000000000000, -0.000000000000000000 ) ) ;
#1935 = CARTESIAN_POINT ( 'NONE',  ( 9.000000000000000000, -3.843229588189086776, -8.684797700342420157 ) ) ;
#1936 = DIRECTION ( 'NONE',  ( 1.000000000000000000, 0.000000000000000000, 0.000000000000000000 ) ) ;
#1937 = EDGE_LOOP ( 'NONE', ( #4559, #1171, #5244, #1501 ) ) ;
#1938 = AXIS2_PLACEMENT_3D ( 'NONE', #184, #596, #2260 ) ;
#1939 = ORIENTED_EDGE ( 'NONE', *, *, #4118, .F. ) ;
#1940 = VECTOR ( 'NONE', #4016, 1000.000000000000227 ) ;
#1941 = SURFACE_SIDE_STYLE ('',( #2367 ) ) ;
#1942 = ORIENTED_EDGE ( 'NONE', *, *, #3391, .F. ) ;
#1943 = DIRECTION ( 'NONE',  ( 0.000000000000000000, 1.000000000000000000, 0.000000000000000000 ) ) ;
#1944 = PLANE ( 'NONE',  #998 ) ;
#1945 = AXIS2_PLACEMENT_3D ( 'NONE', #3613, #5271, #359 ) ;
#1946 =( REPRESENTATION_RELATIONSHIP ('NONE','NONE', #4791, #1634 ) REPRESENTATION_RELATIONSHIP_WITH_TRANSFORMATION ( #5022 )SHAPE_REPRESENTATION_RELATIONSHIP( ) );
#1947 = EDGE_LOOP ( 'NONE', ( #2453, #4214, #4944, #595 ) ) ;
#1948 = AXIS2_PLACEMENT_3D ( 'NONE', #25, #4893, #2807 ) ;
#1949 = CARTESIAN_POINT ( 'NONE',  ( -6.052010058236153789, 6.898175209152294762, -0.1432599722965965938 ) ) ;
#1950 = CARTESIAN_POINT ( 'NONE',  ( -6.403089491455932425, -7.242747656089419728, -9.141698485139452046 ) ) ;
#1951 = PRESENTATION_LAYER_ASSIGNMENT (  '', '', ( #1266 ) ) ;
#1952 = CARTESIAN_POINT ( 'NONE',  ( 6.000000000000000000, 6.009258394948634547E-15, 5.057499999999998330 ) ) ;
#1953 = CYLINDRICAL_SURFACE ( 'NONE', #1809, 5.999999999999950262 ) ;
#1954 = PRODUCT_DEFINITION_SHAPE ( 'NONE', 'NONE',  #4133 ) ;
#1955 = SHAPE_DEFINITION_REPRESENTATION ( #18, #302 ) ;
#1956 = CLOSED_SHELL ( 'NONE', ( #553, #1186, #1833, #3612, #952, #407, #2580, #2460 ) ) ;
#1957 = FACE_OUTER_BOUND ( 'NONE', #514, .T. ) ;
#1958 = VECTOR ( 'NONE', #4709, 1000.000000000000000 ) ;
#1959 = EDGE_CURVE ( 'NONE', #3274, #2898, #4312, .T. ) ;
#1960 = ORIENTED_EDGE ( 'NONE', *, *, #3022, .F. ) ;
#1961 = CARTESIAN_POINT ( 'NONE',  ( 164.0360000000000014, 870.0000000000000000, 6.000000000000005329 ) ) ;
#1962 = ORIENTED_EDGE ( 'NONE', *, *, #4421, .F. ) ;
#1963 =( NAMED_UNIT ( * ) SI_UNIT ( $, .STERADIAN. ) SOLID_ANGLE_UNIT ( ) );
#1964 = LINE ( 'NONE', #3205, #4075 ) ;
#1965 = FACE_OUTER_BOUND ( 'NONE', #2839, .T. ) ;
#1966 = VECTOR ( 'NONE', #3068, 1000.000000000000000 ) ;
#1967 = B_SPLINE_CURVE_WITH_KNOTS ( 'NONE', 3,
 ( #3601, #614, #5256, #1838, #1892, #3219 ),
 .UNSPECIFIED., .F., .F.,
 ( 4, 2, 4 ),
 ( 0.000000000000000000, 0.002769186132444451109, 0.005538372264888902219 ),
 .UNSPECIFIED. ) ;
#1968 = MECHANICAL_DESIGN_GEOMETRIC_PRESENTATION_REPRESENTATION (  '', ( #4732 ), #450 ) ;
#1969 = VERTEX_POINT ( 'NONE', #1199 ) ;
#1970 =( GEOMETRIC_REPRESENTATION_CONTEXT ( 3 ) GLOBAL_UNCERTAINTY_ASSIGNED_CONTEXT ( ( #4081 ) ) GLOBAL_UNIT_ASSIGNED_CONTEXT ( ( #4993, #3756, #1745 ) ) REPRESENTATION_CONTEXT ( 'NONE', 'WORKASPACE' ) );
#1971 = CARTESIAN_POINT ( 'NONE',  ( 75.00000000000001421, 610.0000000000000000, 50.00000000000002132 ) ) ;
#1972 = DIRECTION ( 'NONE',  ( 0.000000000000000000, 1.000000000000000000, -0.000000000000000000 ) ) ;
#1973 = ORIENTED_EDGE ( 'NONE', *, *, #4694, .F. ) ;
#1974 = FILL_AREA_STYLE ('',( #1533 ) ) ;
#1975 = AXIS2_PLACEMENT_3D ( 'NONE', #4462, #331, #4845 ) ;
#1976 = ORIENTED_EDGE ( 'NONE', *, *, #1722, .T. ) ;
#1977 = AXIS2_PLACEMENT_3D ( 'NONE', #2390, #758, #2865 ) ;
#1978 = FILL_AREA_STYLE_COLOUR ( '', #399 ) ;
#1979 = DIRECTION ( 'NONE',  ( 1.000000000000000000, 0.000000000000000000, 2.081668171172168513E-16 ) ) ;
#1980 = EDGE_CURVE ( 'NONE', #2365, #4239, #1415, .T. ) ;
#1981 = ORIENTED_EDGE ( 'NONE', *, *, #3699, .T. ) ;
#1982 = CARTESIAN_POINT ( 'NONE',  ( 6.499999999999993783, 570.0000000000000000, 30.00000000000000711 ) ) ;
#1983 = VECTOR ( 'NONE', #4207, 1000.000000000000000 ) ;
#1984 = EDGE_CURVE ( 'NONE', #4026, #3218, #2480, .T. ) ;
#1985 = ORIENTED_EDGE ( 'NONE', *, *, #2144, .T. ) ;
#1986 = CARTESIAN_POINT ( 'NONE',  ( 121.7157287525372311, -20.00000000000000000, -121.7157287525388369 ) ) ;
#1987 = DIRECTION ( 'NONE',  ( -0.000000000000000000, -1.000000000000000000, -0.000000000000000000 ) ) ;
#1988 = CARTESIAN_POINT ( 'NONE',  ( 0.000000000000000000, 330.0000000000000000, 25.00000000000000000 ) ) ;
#1989 = CARTESIAN_POINT ( 'NONE',  ( -0.4165158504820766772, -10.63278038381084478, -9.021433408186455338 ) ) ;
#1990 = UNCERTAINTY_MEASURE_WITH_UNIT (LENGTH_MEASURE( 1.000000000000000082E-05 ), #1626, 'distance_accuracy_value', 'NONE');
#1991 = SHAPE_DEFINITION_REPRESENTATION ( #1954, #1065 ) ;
#1992 = EDGE_CURVE ( 'NONE', #207, #1147, #312, .T. ) ;
#1993 =( REPRESENTATION_RELATIONSHIP ('NONE','NONE', #4791, #3706 ) REPRESENTATION_RELATIONSHIP_WITH_TRANSFORMATION ( #687 )SHAPE_REPRESENTATION_RELATIONSHIP( ) );
#1994 = FACE_OUTER_BOUND ( 'NONE', #833, .T. ) ;
#1995 = EDGE_LOOP ( 'NONE', ( #3331, #639, #1285, #220 ) ) ;
#1996 = CARTESIAN_POINT ( 'NONE',  ( 0.000000000000000000, 810.0000000000000000, 0.000000000000000000 ) ) ;
#1997 = CARTESIAN_POINT ( 'NONE',  ( 12.00000000000000000, 9.000000000000000000, 0.000000000000000000 ) ) ;
#1998 = DIRECTION ( 'NONE',  ( 0.000000000000000000, 0.000000000000000000, 1.000000000000000000 ) ) ;
#1999 = ORIENTED_EDGE ( 'NONE', *, *, #2888, .T. ) ;
#2000 = ORIENTED_EDGE ( 'NONE', *, *, #4597, .T. ) ;
#2001 = DIRECTION ( 'NONE',  ( 0.000000000000000000, 0.000000000000000000, -1.000000000000000000 ) ) ;
#2002 = PRODUCT_DEFINITION_CONTEXT ( 'detailed design', #3948, 'design' ) ;
#2003 = DIRECTION ( 'NONE',  ( -0.000000000000000000, 1.000000000000000000, -0.000000000000000000 ) ) ;
#2004 = ORIENTED_EDGE ( 'NONE', *, *, #3841, .F. ) ;
#2005 = EDGE_CURVE ( 'NONE', #1160, #2006, #1654, .T. ) ;
#2006 = VERTEX_POINT ( 'NONE', #3768 ) ;
#2007 = EDGE_CURVE ( 'NONE', #5319, #183, #3244, .T. ) ;
#2008 = SURFACE_STYLE_FILL_AREA ( #5317 ) ;
#2009 = PLANE ( 'NONE',  #481 ) ;
#2010 = ORIENTED_EDGE ( 'NONE', *, *, #611, .F. ) ;
#2011 =( LENGTH_UNIT ( ) NAMED_UNIT ( * ) SI_UNIT ( .MILLI., .METRE. ) );
#2012 = ORIENTED_EDGE ( 'NONE', *, *, #1241, .F. ) ;
#2013 = DIRECTION ( 'NONE',  ( -0.9396926207859145341, 0.000000000000000000, -0.3420201433256521151 ) ) ;
#2014 = CARTESIAN_POINT ( 'NONE',  ( -0.7403756379546261313, -10.54036220443003913, -9.525564194215615288 ) ) ;
#2015 = DIRECTION ( 'NONE',  ( -1.000000000000000000, -0.000000000000000000, -0.000000000000000000 ) ) ;
#2016 = DIRECTION ( 'NONE',  ( 0.000000000000000000, 0.000000000000000000, -1.000000000000000000 ) ) ;
#2017 = ITEM_DEFINED_TRANSFORMATION ( 'NONE', 'NONE', #2314,  #4154 ) ;
#2018 = CARTESIAN_POINT ( 'NONE',  ( 6.000000000000000000, 5.839897972853065333, -6.938893903907228378E-15 ) ) ;
#2019 = ORIENTED_EDGE ( 'NONE', *, *, #3681, .T. ) ;
#2020 = CARTESIAN_POINT ( 'NONE',  ( -6.499999999999988454, 390.0000000000000000, 25.00000000000000000 ) ) ;
#2021 =( NAMED_UNIT ( * ) PLANE_ANGLE_UNIT ( ) SI_UNIT ( $, .RADIAN. ) );
#2022 = CARTESIAN_POINT ( 'NONE',  ( -6.245004513516507118E-15, 0.000000000000000000, 30.00000000000001066 ) ) ;
#2023 = CARTESIAN_POINT ( 'NONE',  ( 3.049442433610978414E-16, 10.97743472985185775, -9.686084310752812954 ) ) ;
#2024 = EDGE_LOOP ( 'NONE', ( #1779, #5378, #5038, #249 ) ) ;
#2025 = DIRECTION ( 'NONE',  ( 1.000000000000000000, 0.000000000000000000, 0.000000000000000000 ) ) ;
#2026 = CARTESIAN_POINT ( 'NONE',  ( -5.999999999999999112, 6.928203230275505220, -8.505011083697294083 ) ) ;
#2027 = ORIENTED_EDGE ( 'NONE', *, *, #2727, .T. ) ;
#2028 = ORIENTED_EDGE ( 'NONE', *, *, #4781, .F. ) ;
#2029 = ORIENTED_EDGE ( 'NONE', *, *, #3025, .F. ) ;
#2030 = EDGE_CURVE ( 'NONE', #2382, #813, #1698, .T. ) ;
#2031 = DIRECTION ( 'NONE',  ( 1.000000000000000000, 0.000000000000000000, 0.000000000000000000 ) ) ;
#2032 = VECTOR ( 'NONE', #4152, 1000.000000000000000 ) ;
#2033 = ORIENTED_EDGE ( 'NONE', *, *, #3007, .F. ) ;
#2034 = ORIENTED_EDGE ( 'NONE', *, *, #266, .F. ) ;
#2035 = AXIS2_PLACEMENT_3D ( 'NONE', #3032, #3472, #1764 ) ;
#2036 = VERTEX_POINT ( 'NONE', #3689 ) ;
#2037 = DIRECTION ( 'NONE',  ( -0.000000000000000000, 1.000000000000000000, -0.000000000000000000 ) ) ;
#2038 = DIRECTION ( 'NONE',  ( -0.000000000000000000, -1.000000000000000000, -0.000000000000000000 ) ) ;
#2039 = DIRECTION ( 'NONE',  ( -9.251858538542972814E-17, 0.000000000000000000, 1.000000000000000000 ) ) ;
#2040 = CYLINDRICAL_SURFACE ( 'NONE', #1030, 6.500000000000000000 ) ;
#2041 = AXIS2_PLACEMENT_3D ( 'NONE', #1906, #781, #4085 ) ;
#2042 = UNCERTAINTY_MEASURE_WITH_UNIT (LENGTH_MEASURE( 1.000000000000000082E-05 ), #4102, 'distance_accuracy_value', 'NONE');
#2043 = APPLICATION_PROTOCOL_DEFINITION ( 'draft international standard', 'automotive_design', 1998, #2066 ) ;
#2044 = VECTOR ( 'NONE', #4121, 1000.000000000000000 ) ;
#2045 = DIRECTION ( 'NONE',  ( 0.000000000000000000, 0.5000000000000008882, 0.8660254037844381525 ) ) ;
#2046 = ORIENTED_EDGE ( 'NONE', *, *, #3190, .T. ) ;
#2047 = CARTESIAN_POINT ( 'NONE',  ( 25.00000000000000355, 10.00000000000000000, 25.00000000000000000 ) ) ;
#2048 =( LENGTH_UNIT ( ) NAMED_UNIT ( * ) SI_UNIT ( .MILLI., .METRE. ) );
#2049 = CLOSED_SHELL ( 'NONE', ( #1815, #2075, #5383, #2874, #1275, #1509, #4252, #1653, #3658, #4584, #4343, #911, #3183, #4050, #2401, #4954 ) ) ;
#2050 = DIRECTION ( 'NONE',  ( -0.000000000000000000, -0.000000000000000000, 1.000000000000000000 ) ) ;
#2051 = ADVANCED_FACE ( 'NONE', ( #1165 ), #2929, .F. ) ;
#2052 = CARTESIAN_POINT ( 'NONE',  ( 0.000000000000000000, 390.0000000000000000, -25.00000000000000000 ) ) ;
#2053 = PRODUCT_DEFINITION_FORMATION_WITH_SPECIFIED_SOURCE ( 'ANY', '', #2638, .NOT_KNOWN. ) ;
#2054 = VECTOR ( 'NONE', #2249, 1000.000000000000000 ) ;
#2055 =( GEOMETRIC_REPRESENTATION_CONTEXT ( 3 ) GLOBAL_UNCERTAINTY_ASSIGNED_CONTEXT ( ( #2829 ) ) GLOBAL_UNIT_ASSIGNED_CONTEXT ( ( #2615, #1028, #3840 ) ) REPRESENTATION_CONTEXT ( 'NONE', 'WORKASPACE' ) );
#2056 = ADVANCED_FACE ( 'NONE', ( #2840 ), #843, .F. ) ;
#2057 = CIRCLE ( 'NONE', #140, 5.035999999999999588 ) ;
#2058 = ORIENTED_EDGE ( 'NONE', *, *, #3438, .T. ) ;
#2059 = DIRECTION ( 'NONE',  ( 1.000000000000000000, 0.000000000000000000, 0.000000000000000000 ) ) ;
#2060 = CARTESIAN_POINT ( 'NONE',  ( 0.000000000000000000, 0.000000000000000000, -0.6301867843887398735 ) ) ;
#2061 = VERTEX_POINT ( 'NONE', #4174 ) ;
#2062 = ORIENTED_EDGE ( 'NONE', *, *, #5162, .F. ) ;
#2063 = AXIS2_PLACEMENT_3D ( 'NONE', #3735, #5075, #89 ) ;
#2064 = DIRECTION ( 'NONE',  ( 0.000000000000000000, 0.000000000000000000, -1.000000000000000000 ) ) ;
#2065 = VERTEX_POINT ( 'NONE', #2432 ) ;
#2066 = APPLICATION_CONTEXT ( 'automotive_design' ) ;
#2067 = EDGE_CURVE ( 'NONE', #165, #2036, #4515, .T. ) ;
#2068 = AXIS2_PLACEMENT_3D ( 'NONE', #812, #4268, #114 ) ;
#2069 = EDGE_CURVE ( 'NONE', #4480, #4433, #1370, .T. ) ;
#2070 = ORIENTED_EDGE ( 'NONE', *, *, #2170, .T. ) ;
#2071 = CARTESIAN_POINT ( 'NONE',  ( 6.757601037695092606E-16, 840.0000000000001137, 5.035999999999999588 ) ) ;
#2072 = CARTESIAN_POINT ( 'NONE',  ( -2.822677224501521920, 8.762631390013995158, -8.969375302471101818 ) ) ;
#2073 = CARTESIAN_POINT ( 'NONE',  ( 1.171714802207676431, -9.715814988945201236, -8.684787165853032675 ) ) ;
#2074 = VECTOR ( 'NONE', #3618, 1000.000000000000000 ) ;
#2075 = ADVANCED_FACE ( 'NONE', ( #868 ), #3866, .F. ) ;
#2076 = EDGE_CURVE ( 'NONE', #2978, #1856, #4066, .T. ) ;
#2077 = ORIENTED_EDGE ( 'NONE', *, *, #3783, .T. ) ;
#2078 = CARTESIAN_POINT ( 'NONE',  ( 1.410908427127813464E-14, 582.4999999999997726, 50.00000000000000000 ) ) ;
#2079 = CARTESIAN_POINT ( 'NONE',  ( 164.0360000000000014, 870.0000000000000000, 0.000000000000000000 ) ) ;
#2080 = DIRECTION ( 'NONE',  ( -0.000000000000000000, -0.000000000000000000, 1.000000000000000000 ) ) ;
#2081 = CARTESIAN_POINT ( 'NONE',  ( -9.000000000000000000, -3.792382572872301072, -8.707340555897303602 ) ) ;
#2082 = ORIENTED_EDGE ( 'NONE', *, *, #1081, .T. ) ;
#2083 = ORIENTED_EDGE ( 'NONE', *, *, #4792, .F. ) ;
#2084 = CARTESIAN_POINT ( 'NONE',  ( 1.538998812063697930, 10.06940755529822695, -9.383905213720977301 ) ) ;
#2085 = CARTESIAN_POINT ( 'NONE',  ( 9.000000000000000000, 0.4512186429437704538, -0.007346088320835161140 ) ) ;
#2086 = EDGE_LOOP ( 'NONE', ( #927, #2033 ) ) ;
#2087 = ORIENTED_EDGE ( 'NONE', *, *, #3943, .F. ) ;
#2088 = ORIENTED_EDGE ( 'NONE', *, *, #1292, .F. ) ;
#2089 = CARTESIAN_POINT ( 'NONE',  ( 165.0000000000000000, 870.0000000000000000, 0.000000000000000000 ) ) ;
#2090 = ORIENTED_EDGE ( 'NONE', *, *, #2811, .F. ) ;
#2091 = EDGE_CURVE ( 'NONE', #5063, #3611, #2129, .T. ) ;
#2092 = ORIENTED_EDGE ( 'NONE', *, *, #1580, .T. ) ;
#2093 = CARTESIAN_POINT ( 'NONE',  ( -150.0000000000000000, 870.0000000000000000, -5.999999999999950262 ) ) ;
#2094 = DIRECTION ( 'NONE',  ( -0.000000000000000000, -1.000000000000000000, -0.000000000000000000 ) ) ;
#2095 = CARTESIAN_POINT ( 'NONE',  ( -7.546085493343360540, -6.035570354503548174, -0.5405968996908985247 ) ) ;
#2096 = ORIENTED_EDGE ( 'NONE', *, *, #3480, .T. ) ;
#2097 = PLANE ( 'NONE',  #4906 ) ;
#2098 = DIRECTION ( 'NONE',  ( 0.000000000000000000, 0.000000000000000000, -1.000000000000000000 ) ) ;
#2099 = LINE ( 'NONE', #4994, #3097 ) ;
#2100 = EDGE_CURVE ( 'NONE', #4209, #3573, #395, .T. ) ;
#2101 = CARTESIAN_POINT ( 'NONE',  ( -9.000000000000000000, 1.973624059910456197, -8.465093423469367551 ) ) ;
#2102 = ORIENTED_EDGE ( 'NONE', *, *, #79, .T. ) ;
#2103 = VERTEX_POINT ( 'NONE', #3021 ) ;
#2104 = CARTESIAN_POINT ( 'NONE',  ( 0.7403756379549473188, 10.54036220443051874, -9.525564194215789371 ) ) ;
#2105 = CARTESIAN_POINT ( 'NONE',  ( 9.000000000000001776, 1.123146974283612654, -0.05788585198792846331 ) ) ;
#2106 = EDGE_LOOP ( 'NONE', ( #320, #863, #3687, #1031 ) ) ;
#2107 = ORIENTED_EDGE ( 'NONE', *, *, #521, .F. ) ;
#2108 = CARTESIAN_POINT ( 'NONE',  ( 4.500000000000003553, -7.794228634059947147, 0.000000000000000000 ) ) ;
#2109 = ORIENTED_EDGE ( 'NONE', *, *, #2872, .F. ) ;
#2110 =( NAMED_UNIT ( * ) PLANE_ANGLE_UNIT ( ) SI_UNIT ( $, .RADIAN. ) );
#2111 = ORIENTED_EDGE ( 'NONE', *, *, #5360, .T. ) ;
#2112 = PRODUCT_RELATED_PRODUCT_CATEGORY ( 'part', '', ( #313 ) ) ;
#2113 = AXIS2_PLACEMENT_3D ( 'NONE', #1923, #1512, #4872 ) ;
#2114 = VERTEX_POINT ( 'NONE', #1811 ) ;
#2115 = FACE_BOUND ( 'NONE', #772, .T. ) ;
#2116 = CARTESIAN_POINT ( 'NONE',  ( 25.00000000000000000, 810.0000000000000000, 25.00000000000000711 ) ) ;
#2117 = CARTESIAN_POINT ( 'NONE',  ( -9.000000000000000000, -5.196152422706636465, -1.199999999999999734 ) ) ;
#2118 = CONTEXT_DEPENDENT_SHAPE_REPRESENTATION ( #1946, #4276 ) ;
#2119 = AXIS2_PLACEMENT_3D ( 'NONE', #5170, #3491, #2753 ) ;
#2120 = DIRECTION ( 'NONE',  ( 1.000000000000000000, 0.000000000000000000, 0.000000000000000000 ) ) ;
#2121 = AXIS2_PLACEMENT_3D ( 'NONE', #4524, #1519, #4027 ) ;
#2122 = EDGE_LOOP ( 'NONE', ( #2653, #5131, #3837, #5147, #3884 ) ) ;
#2123 = DIRECTION ( 'NONE',  ( -1.000000000000000000, -0.000000000000000000, -0.000000000000000000 ) ) ;
#2124 = CARTESIAN_POINT ( 'NONE',  ( -4.500000000000002665, -7.794228634059946259, 0.000000000000000000 ) ) ;
#2125 = DIRECTION ( 'NONE',  ( 1.000000000000000000, 0.000000000000000000, 0.000000000000000000 ) ) ;
#2126 = FACE_OUTER_BOUND ( 'NONE', #1735, .T. ) ;
#2127 =( NAMED_UNIT ( * ) PLANE_ANGLE_UNIT ( ) SI_UNIT ( $, .RADIAN. ) );
#2128 = EDGE_CURVE ( 'NONE', #3079, #2174, #2998, .T. ) ;
#2129 = CIRCLE ( 'NONE', #2748, 12.38940648156203927 ) ;
#2130 = CARTESIAN_POINT ( 'NONE',  ( 6.000000000000000000, 2.919948986426526005, -5.057500000000002771 ) ) ;
#2131 = AXIS2_PLACEMENT_3D ( 'NONE', #187, #2711, #1845 ) ;
#2132 = DIRECTION ( 'NONE',  ( 0.000000000000000000, 0.000000000000000000, 1.000000000000000000 ) ) ;
#2133 = LINE ( 'NONE', #5002, #1444 ) ;
#2134 = CONICAL_SURFACE ( 'NONE', #4922, 9.000000000000001776, 0.8594454914424796144 ) ;
#2135 = ORIENTED_EDGE ( 'NONE', *, *, #52, .T. ) ;
#2136 = EDGE_CURVE ( 'NONE', #1856, #3771, #2563, .T. ) ;
#2137 = CIRCLE ( 'NONE', #4158, 12.07201791628681420 ) ;
#2138 = STYLED_ITEM ( 'NONE', ( #1873 ), #4176 ) ;
#2139 = PRODUCT ( 'axle', 'axle', '', ( #3254 ) ) ;
#2140 = CARTESIAN_POINT ( 'NONE',  ( -150.0000000000000000, 810.0000000000000000, 25.00000000000000000 ) ) ;
#2141 = SURFACE_STYLE_FILL_AREA ( #2457 ) ;
#2142 = CIRCLE ( 'NONE', #2860, 5.999999999999950262 ) ;
#2143 = COLOUR_RGB ( '',0.8941176470588234615, 0.8941176470588234615, 0.8941176470588234615 ) ;
#2144 = EDGE_CURVE ( 'NONE', #3920, #4400, #2299, .T. ) ;
#2145 = VECTOR ( 'NONE', #3400, 1000.000000000000000 ) ;
#2146 = VERTEX_POINT ( 'NONE', #2537 ) ;
#2147 = DIRECTION ( 'NONE',  ( 1.000000000000000000, -0.000000000000000000, -0.000000000000000000 ) ) ;
#2148 = DIRECTION ( 'NONE',  ( 0.000000000000000000, -1.000000000000000000, 0.000000000000000000 ) ) ;
#2149 = CARTESIAN_POINT ( 'NONE',  ( -9.564083412974085263, 5.456344092479594288, -9.698321917585790430 ) ) ;
#2150 = DIRECTION ( 'NONE',  ( -1.000000000000000000, -0.000000000000000000, -0.000000000000000000 ) ) ;
#2151 = EDGE_CURVE ( 'NONE', #457, #3895, #836, .T. ) ;
#2152 = AXIS2_PLACEMENT_3D ( 'NONE', #607, #2274, #3536 ) ;
#2153 = FACE_OUTER_BOUND ( 'NONE', #1589, .T. ) ;
#2154 = DIRECTION ( 'NONE',  ( 1.000000000000000000, 0.000000000000000000, 0.000000000000000000 ) ) ;
#2155 = DIRECTION ( 'NONE',  ( 0.000000000000000000, 0.000000000000000000, -1.000000000000000000 ) ) ;
#2156 = VECTOR ( 'NONE', #1547, 1000.000000000000000 ) ;
#2157 = DIRECTION ( 'NONE',  ( -0.000000000000000000, -0.000000000000000000, -1.000000000000000000 ) ) ;
#2158 = EDGE_LOOP ( 'NONE', ( #1743, #3423, #235, #2077 ) ) ;
#2159 = CARTESIAN_POINT ( 'NONE',  ( -9.000000000000000000, -0.9276453582363817230, -8.460808235231727537 ) ) ;
#2160 = EDGE_CURVE ( 'NONE', #1561, #4335, #4227, .T. ) ;
#2161 = CIRCLE ( 'NONE', #2880, 6.499999999999988454 ) ;
#2162 = VECTOR ( 'NONE', #2123, 1000.000000000000000 ) ;
#2163 = EDGE_LOOP ( 'NONE', ( #671, #276, #2307, #5328 ) ) ;
#2164 = SURFACE_STYLE_USAGE ( .BOTH. , #3406 ) ;
#2165 = CARTESIAN_POINT ( 'NONE',  ( 9.562637692001345613, 5.457160213363109413, -9.698012095152311218 ) ) ;
#2166 = CARTESIAN_POINT ( 'NONE',  ( 6.499999999999993783, 570.0000000000000000, 25.00000000000000000 ) ) ;
#2167 = APPLICATION_CONTEXT ( 'automotive_design' ) ;
#2168 = CARTESIAN_POINT ( 'NONE',  ( 9.000000000000001776, -5.196152422706638241, -1.199999999999999734 ) ) ;
#2169 = EDGE_CURVE ( 'NONE', #963, #366, #2579, .T. ) ;
#2170 = EDGE_CURVE ( 'NONE', #165, #503, #3892, .T. ) ;
#2171 = ORIENTED_EDGE ( 'NONE', *, *, #2005, .F. ) ;
#2172 = EDGE_LOOP ( 'NONE', ( #1273, #3625, #2342, #2767 ) ) ;
#2173 = DIRECTION ( 'NONE',  ( 1.000000000000000000, 0.000000000000000000, 0.000000000000000000 ) ) ;
#2174 = VERTEX_POINT ( 'NONE', #149 ) ;
#2175 = FACE_OUTER_BOUND ( 'NONE', #674, .T. ) ;
#2176 = DIRECTION ( 'NONE',  ( 1.000000000000000000, 0.000000000000000000, 0.000000000000000000 ) ) ;
#2177 = CONTEXT_DEPENDENT_SHAPE_REPRESENTATION ( #3533, #2809 ) ;
#2178 =( BOUNDED_SURFACE ( )  B_SPLINE_SURFACE ( 3, 2, ( 
 ( #1989, #86, #1252 ),
 ( #2073, #4545, #4156 ),
 ( #2465, #492, #4129 ),
 ( #892, #3729, #2963 ),
 ( #1660, #5382, #2981 ),
 ( #3005, #1741, #824 ),
 ( #378, #5046, #3418 ),
 ( #31, #5069, #3339 ) ),
 .UNSPECIFIED., .F., .F., .T. ) 
 B_SPLINE_SURFACE_WITH_KNOTS ( ( 4, 2, 2, 4 ),
 ( 3, 3 ),
 ( 0.04613854442509285336, 0.05169925677048779755, 0.05447961294318526965, 0.05725996911588274174 ),
 ( 0.000000000000000000, 1.000000000000000000 ),
 .UNSPECIFIED. ) 
 GEOMETRIC_REPRESENTATION_ITEM ( )  RATIONAL_B_SPLINE_SURFACE ( (
 ( 1.000000000000000000, 0.8047781684971944127, 1.000000000000000000),
 ( 1.000000000000000000, 0.8123765127742887948, 1.000000000000000000),
 ( 1.000000000000000000, 0.8190661184400637174, 1.000000000000000000),
 ( 1.000000000000000000, 0.8191936944252291575, 1.000000000000000000),
 ( 1.000000000000000000, 0.8176092056339582248, 1.000000000000000000),
 ( 1.000000000000000000, 0.8122961334886901197, 1.000000000000000000),
 ( 1.000000000000000000, 0.8086310951057499308, 1.000000000000000000),
 ( 1.000000000000000000, 0.8047712311394933371, 1.000000000000000000) ) ) 
 REPRESENTATION_ITEM ( '' )  SURFACE ( )  );
#2179 = LINE ( 'NONE', #5123, #3715 ) ;
#2180 = ORIENTED_EDGE ( 'NONE', *, *, #3245, .T. ) ;
#2181 = CARTESIAN_POINT ( 'NONE',  ( 9.489636812669466792, -3.671909760406012246, -9.380312854821335478 ) ) ;
#2182 = DIRECTION ( 'NONE',  ( 0.000000000000000000, 0.000000000000000000, 1.000000000000000000 ) ) ;
#2183 = DIRECTION ( 'NONE',  ( -1.000000000000000000, 0.000000000000000000, 0.000000000000000000 ) ) ;
#2184 = CARTESIAN_POINT ( 'NONE',  ( 6.499999999999986677, 35.00000000000000000, 30.00000000000000711 ) ) ;
#2185 = SURFACE_STYLE_USAGE ( .BOTH. , #2578 ) ;
#2186 = AXIS2_PLACEMENT_3D ( 'NONE', #3964, #4419, #3938 ) ;
#2187 = ORIENTED_EDGE ( 'NONE', *, *, #3722, .T. ) ;
#2188 = PRODUCT_DEFINITION ( 'UNKNOWN', '', #1092, #5338 ) ;
#2189 = EDGE_LOOP ( 'NONE', ( #2549, #4188, #2720, #296 ) ) ;
#2190 = LINE ( 'NONE', #4683, #1917 ) ;
#2191 = CARTESIAN_POINT ( 'NONE',  ( 3.715604115503464921, 8.247099809125259640, -0.03002505116510094385 ) ) ;
#2192 = CARTESIAN_POINT ( 'NONE',  ( 1.272360546691145400, 9.657707141273826679, -9.220334578152899141 ) ) ;
#2193 = DIRECTION ( 'NONE',  ( -0.000000000000000000, -0.000000000000000000, 1.000000000000000000 ) ) ;
#2194 = DIRECTION ( 'NONE',  ( 0.000000000000000000, -1.000000000000000000, 0.000000000000000000 ) ) ;
#2195 = ADVANCED_FACE ( 'NONE', ( #4216 ), #1756, .T. ) ;
#2196 = EDGE_LOOP ( 'NONE', ( #1942, #384 ) ) ;
#2197 = CARTESIAN_POINT ( 'NONE',  ( -165.0000000000000000, 870.0000000000000000, 0.000000000000000000 ) ) ;
#2198 = CARTESIAN_POINT ( 'NONE',  ( 0.6000000000000033085, 0.000000000000000000, 9.000000000000000000 ) ) ;
#2199 = DIRECTION ( 'NONE',  ( -1.000000000000000000, -0.000000000000000000, -0.000000000000000000 ) ) ;
#2200 = B_SPLINE_CURVE_WITH_KNOTS ( 'NONE', 3,
 ( #1430, #3112, #4756, #4045, #1949, #683, #4358, #4784 ),
 .UNSPECIFIED., .F., .F.,
 ( 4, 2, 2, 4 ),
 ( 2.475501736920113682E-07, 0.002666746755945494790, 0.003999996358831395607, 0.005333245961717295557 ),
 .UNSPECIFIED. ) ;
#2201 = CARTESIAN_POINT ( 'NONE',  ( 0.000000000000000000, 0.000000000000000000, -12.00000000000000178 ) ) ;
#2202 = EDGE_LOOP ( 'NONE', ( #1268, #451, #4763, #1564 ) ) ;
#2203 = DIRECTION ( 'NONE',  ( -1.000000000000000000, -7.401486830834378251E-16, -2.081668171172168513E-16 ) ) ;
#2204 =( LENGTH_UNIT ( ) NAMED_UNIT ( * ) SI_UNIT ( .MILLI., .METRE. ) );
#2205 = DIRECTION ( 'NONE',  ( 0.000000000000000000, -1.000000000000000000, 0.000000000000000000 ) ) ;
#2206 = CARTESIAN_POINT ( 'NONE',  ( -74.99999999999998579, 610.0000000000000000, 29.99999999999999289 ) ) ;
#2207 = CONICAL_SURFACE ( 'NONE', #2930, 5.036000000000040444, 0.7853981633974339571 ) ;
#2208 = ADVANCED_BREP_SHAPE_REPRESENTATION ( '', ( #258, #4154 ), #2227 ) ;
#2209 = CARTESIAN_POINT ( 'NONE',  ( -2.411623992625733778E-15, 35.00000000000000000, 42.00000000000000000 ) ) ;
#2210 = AXIS2_PLACEMENT_3D ( 'NONE', #1364, #3526, #5185 ) ;
#2211 = EDGE_CURVE ( 'NONE', #2280, #4026, #3387, .T. ) ;
#2212 = PLANE ( 'NONE',  #3440 ) ;
#2213 = VERTEX_POINT ( 'NONE', #117 ) ;
#2214 = DIRECTION ( 'NONE',  ( 0.000000000000000000, -1.000000000000000000, 1.039664082171044284E-15 ) ) ;
#2215 = DIRECTION ( 'NONE',  ( -0.000000000000000000, -1.000000000000000000, -0.000000000000000000 ) ) ;
#2216 = LINE ( 'NONE', #146, #3281 ) ;
#2217 = CARTESIAN_POINT ( 'NONE',  ( 0.000000000000000000, 839.0360000000000582, 0.000000000000000000 ) ) ;
#2218 = ADVANCED_FACE ( 'NONE', ( #1318 ), #4636, .T. ) ;
#2219 = VECTOR ( 'NONE', #1271, 1000.000000000000000 ) ;
#2220 = DIRECTION ( 'NONE',  ( -0.000000000000000000, -0.000000000000000000, 1.000000000000000000 ) ) ;
#2221 = CIRCLE ( 'NONE', #2587, 6.499999999999999112 ) ;
#2222 = VECTOR ( 'NONE', #2842, 1000.000000000000000 ) ;
#2223 = ORIENTED_EDGE ( 'NONE', *, *, #2169, .T. ) ;
#2224 = CARTESIAN_POINT ( 'NONE',  ( -9.489636812669466792, 3.671909760406011358, -9.380312854821335478 ) ) ;
#2225 = CIRCLE ( 'NONE', #2947, 6.000000000000000888 ) ;
#2226 = CARTESIAN_POINT ( 'NONE',  ( -30.00000000000000355, 610.0000000000000000, -2.081668171172168908E-15 ) ) ;
#2227 =( GEOMETRIC_REPRESENTATION_CONTEXT ( 3 ) GLOBAL_UNCERTAINTY_ASSIGNED_CONTEXT ( ( #757 ) ) GLOBAL_UNIT_ASSIGNED_CONTEXT ( ( #1560, #4036, #1134 ) ) REPRESENTATION_CONTEXT ( 'NONE', 'WORKASPACE' ) );
#2228 = CARTESIAN_POINT ( 'NONE',  ( -150.0000000000000000, 810.0000000000000000, -25.00000000000000000 ) ) ;
#2229 = VECTOR ( 'NONE', #3421, 1000.000000000000000 ) ;
#2230 = PRESENTATION_LAYER_ASSIGNMENT (  '', '', ( #3546 ) ) ;
#2231 = ORIENTED_EDGE ( 'NONE', *, *, #742, .F. ) ;
#2232 = ORIENTED_EDGE ( 'NONE', *, *, #5241, .F. ) ;
#2233 = CYLINDRICAL_SURFACE ( 'NONE', #3417, 6.499999999999983125 ) ;
#2234 = CARTESIAN_POINT ( 'NONE',  ( -5.099999999999999645, 6.245698675651500839E-16, -0.6301867843887398735 ) ) ;
#2235 = CARTESIAN_POINT ( 'NONE',  ( 6.499999999999988454, 450.0000000000000000, 25.00000000000000000 ) ) ;
#2236 = ORIENTED_EDGE ( 'NONE', *, *, #139, .T. ) ;
#2237 = EDGE_CURVE ( 'NONE', #1195, #4535, #1778, .T. ) ;
#2238 = CARTESIAN_POINT ( 'NONE',  ( 92.00000000000000000, 0.000000000000000000, 5.035999999999999588 ) ) ;
#2239 = CIRCLE ( 'NONE', #1018, 6.000000000000005329 ) ;
#2240 = EDGE_CURVE ( 'NONE', #5253, #850, #5182, .T. ) ;
#2241 = TOROIDAL_SURFACE ( 'NONE', #3743, 8.400000000000000355, 0.5999999999999999778 ) ;
#2242 = CARTESIAN_POINT ( 'NONE',  ( 139.9999999999999716, 885.0000000000000000, 25.00000000000000000 ) ) ;
#2243 = LINE ( 'NONE', #983, #2627 ) ;
#2244 = LINE ( 'NONE', #171, #1278 ) ;
#2245 = DIRECTION ( 'NONE',  ( -0.000000000000000000, 1.000000000000000000, -0.000000000000000000 ) ) ;
#2246 = CARTESIAN_POINT ( 'NONE',  ( 6.499999999999988454, 330.0000000000000000, -25.00000000000000000 ) ) ;
#2247 = ORIENTED_EDGE ( 'NONE', *, *, #2067, .T. ) ;
#2248 = AXIS2_PLACEMENT_3D ( 'NONE', #3992, #3161, #1175 ) ;
#2249 = DIRECTION ( 'NONE',  ( -0.000000000000000000, -1.000000000000000000, -0.000000000000000000 ) ) ;
#2250 = DIRECTION ( 'NONE',  ( 1.000000000000000000, 0.000000000000000000, 0.000000000000000000 ) ) ;
#2251 =( NAMED_UNIT ( * ) PLANE_ANGLE_UNIT ( ) SI_UNIT ( $, .RADIAN. ) );
#2252 = VERTEX_POINT ( 'NONE', #195 ) ;
#2253 = ADVANCED_FACE ( 'NONE', ( #1104 ), #2541, .F. ) ;
#2254 = SURFACE_STYLE_USAGE ( .BOTH. , #1941 ) ;
#2255 = DIRECTION ( 'NONE',  ( 0.000000000000000000, 0.000000000000000000, 1.000000000000000000 ) ) ;
#2256 = DIRECTION ( 'NONE',  ( -0.000000000000000000, -1.000000000000000000, -0.000000000000000000 ) ) ;
#2257 = CONICAL_SURFACE ( 'NONE', #6, 9.000000000000001776, 0.8594454914424796144 ) ;
#2258 = ORIENTED_EDGE ( 'NONE', *, *, #1580, .F. ) ;
#2259 = ORIENTED_EDGE ( 'NONE', *, *, #4401, .T. ) ;
#2260 = DIRECTION ( 'NONE',  ( 0.000000000000000000, 0.000000000000000000, -1.000000000000000000 ) ) ;
#2261 = FACE_BOUND ( 'NONE', #4304, .T. ) ;
#2262 = FACE_BOUND ( 'NONE', #3264, .T. ) ;
#2263 = DIRECTION ( 'NONE',  ( 1.000000000000000000, 0.000000000000000000, 0.000000000000000000 ) ) ;
#2264 = SHAPE_REPRESENTATION_RELATIONSHIP ( 'NONE' , 'NONE' ,  #2934, #4176 ) ;
#2265 = EDGE_CURVE ( 'NONE', #3572, #2394, #217, .T. ) ;
#2266 = ADVANCED_FACE ( 'NONE', ( #3150 ), #2331, .F. ) ;
#2267 = CARTESIAN_POINT ( 'NONE',  ( 149.9999999999999716, 10.00000000000000000, 149.9999999999999716 ) ) ;
#2268 = LINE ( 'NONE', #1438, #3844 ) ;
#2269 = DIRECTION ( 'NONE',  ( -0.7071067811865482389, 8.659560562354941486E-17, 0.7071067811865469066 ) ) ;
#2270 = CYLINDRICAL_SURFACE ( 'NONE', #3188, 6.499999999999988454 ) ;
#2271 = DIRECTION ( 'NONE',  ( -1.000000000000000000, 0.000000000000000000, 0.000000000000000000 ) ) ;
#2272 = PRODUCT_DEFINITION_SHAPE ( 'NONE', 'NONE',  #5393 ) ;
#2273 = LINE ( 'NONE', #2360, #2755 ) ;
#2274 = DIRECTION ( 'NONE',  ( 0.000000000000000000, -1.000000000000000000, 0.000000000000000000 ) ) ;
#2275 = ORIENTED_EDGE ( 'NONE', *, *, #5054, .T. ) ;
#2276 = EDGE_LOOP ( 'NONE', ( #1221, #1921, #369, #3384 ) ) ;
#2277 = ORIENTED_EDGE ( 'NONE', *, *, #4271, .F. ) ;
#2278 = FACE_OUTER_BOUND ( 'NONE', #4065, .T. ) ;
#2279 = EDGE_CURVE ( 'NONE', #4279, #2394, #1024, .T. ) ;
#2280 = VERTEX_POINT ( 'NONE', #2664 ) ;
#2281 = LINE ( 'NONE', #4377, #300 ) ;
#2282 = LINE ( 'NONE', #4671, #3311 ) ;
#2283 = EDGE_CURVE ( 'NONE', #4388, #3602, #282, .T. ) ;
#2284 = PRODUCT_RELATED_PRODUCT_CATEGORY ( 'part', '', ( #2638 ) ) ;
#2285 = ORIENTED_EDGE ( 'NONE', *, *, #1755, .F. ) ;
#2286 = ORIENTED_EDGE ( 'NONE', *, *, #1399, .T. ) ;
#2287 = ORIENTED_EDGE ( 'NONE', *, *, #1594, .T. ) ;
#2288 = CARTESIAN_POINT ( 'NONE',  ( 3.049442433610978414E-16, 10.97743472985185775, -9.686084310752812954 ) ) ;
#2289 = CARTESIAN_POINT ( 'NONE',  ( -9.000000000000000000, 5.196152422706629359, -12.00000000000000000 ) ) ;
#2290 = FACE_OUTER_BOUND ( 'NONE', #2869, .T. ) ;
#2291 = DIRECTION ( 'NONE',  ( 1.000000000000000000, 0.000000000000000000, 0.000000000000000000 ) ) ;
#2292 = EDGE_LOOP ( 'NONE', ( #1868, #3111, #2396 ) ) ;
#2293 = LINE ( 'NONE', #3453, #4061 ) ;
#2294 = AXIS2_PLACEMENT_3D ( 'NONE', #4960, #4519, #354 ) ;
#2295 = FACE_OUTER_BOUND ( 'NONE', #682, .T. ) ;
#2296 = LINE ( 'NONE', #3090, #849 ) ;
#2297 = DIRECTION ( 'NONE',  ( 0.000000000000000000, 0.000000000000000000, -1.000000000000000000 ) ) ;
#2298 = ADVANCED_FACE ( 'NONE', ( #4324 ), #3595, .T. ) ;
#2299 = B_SPLINE_CURVE_WITH_KNOTS ( 'NONE', 3,
 ( #2168, #5062, #887, #532, #3049, #3487, #2956, #2108 ),
 .UNSPECIFIED., .F., .F.,
 ( 4, 2, 2, 4 ),
 ( 2.475501736915396238E-07, 0.002666746755945493055, 0.003999996358831392138, 0.005333245961717292087 ),
 .UNSPECIFIED. ) ;
#2300 = AXIS2_PLACEMENT_3D ( 'NONE', #1326, #1687, #4649 ) ;
#2301 = CARTESIAN_POINT ( 'NONE',  ( 9.000000000000000000, 0.9093366823532084142, -8.964884200296355132 ) ) ;
#2302 = CARTESIAN_POINT ( 'NONE',  ( 5.099999999999999645, 0.000000000000000000, -12.00000000000000000 ) ) ;
#2303 = AXIS2_PLACEMENT_3D ( 'NONE', #100, #4300, #2173 ) ;
#2304 = ORIENTED_EDGE ( 'NONE', *, *, #3972, .T. ) ;
#2305 = EDGE_CURVE ( 'NONE', #353, #4898, #2273, .T. ) ;
#2306 = CIRCLE ( 'NONE', #4646, 5.036000000000040444 ) ;
#2307 = ORIENTED_EDGE ( 'NONE', *, *, #688, .F. ) ;
#2308 = LINE ( 'NONE', #4014, #2663 ) ;
#2309 =( REPRESENTATION_RELATIONSHIP ('NONE','NONE', #4791, #2934 ) REPRESENTATION_RELATIONSHIP_WITH_TRANSFORMATION ( #3340 )SHAPE_REPRESENTATION_RELATIONSHIP( ) );
#2310 = ORIENTED_EDGE ( 'NONE', *, *, #563, .T. ) ;
#2311 = CARTESIAN_POINT ( 'NONE',  ( -164.0360000000000014, 870.0000000000000000, -6.000000000000006217 ) ) ;
#2312 = EDGE_CURVE ( 'NONE', #2368, #1147, #4398, .T. ) ;
#2313 = CIRCLE ( 'NONE', #913, 6.000000000000006217 ) ;
#2314 = AXIS2_PLACEMENT_3D ( 'NONE', #4311, #3141, #2734 ) ;
#2315 = ORIENTED_EDGE ( 'NONE', *, *, #3447, .T. ) ;
#2316 = CARTESIAN_POINT ( 'NONE',  ( -165.0000000000000000, 870.0000000000000000, 5.036000000000040444 ) ) ;
#2317 = CARTESIAN_POINT ( 'NONE',  ( -7.828285197792963501, -5.872642279174337787, -8.684787165848932844 ) ) ;
#2318 = LINE ( 'NONE', #3552, #4927 ) ;
#2319 = CARTESIAN_POINT ( 'NONE',  ( -1.676835913137321903E-15, 35.00000000000000000, 30.00000000000000711 ) ) ;
#2320 = CARTESIAN_POINT ( 'NONE',  ( 0.000000000000000000, 0.000000000000000000, 0.000000000000000000 ) ) ;
#2321 = CIRCLE ( 'NONE', #3024, 6.499999999999988454 ) ;
#2322 = AXIS2_PLACEMENT_3D ( 'NONE', #144, #1384, #1366 ) ;
#2323 = CARTESIAN_POINT ( 'NONE',  ( 0.000000000000000000, 0.000000000000000000, -11.07201791628681775 ) ) ;
#2324 = VERTEX_POINT ( 'NONE', #3507 ) ;
#2325 = CARTESIAN_POINT ( 'NONE',  ( 92.00000000000000000, 0.000000000000000000, 0.000000000000000000 ) ) ;
#2326 = CARTESIAN_POINT ( 'NONE',  ( -7.921880722261733787, 6.383959649155158900, -9.379910571084323578 ) ) ;
#2327 = ADVANCED_FACE ( 'NONE', ( #1498 ), #3173, .F. ) ;
#2328 = DIRECTION ( 'NONE',  ( -0.000000000000000000, -1.000000000000000000, -0.000000000000000000 ) ) ;
#2329 = PRODUCT_DEFINITION_CONTEXT ( 'detailed design', #2921, 'design' ) ;
#2330 = DIRECTION ( 'NONE',  ( -0.000000000000000000, -0.000000000000000000, 1.000000000000000000 ) ) ;
#2331 = PLANE ( 'NONE',  #2412 ) ;
#2332 = DIRECTION ( 'NONE',  ( 0.000000000000000000, 0.000000000000000000, 1.000000000000000000 ) ) ;
#2333 = AXIS2_PLACEMENT_3D ( 'NONE', #3196, #1121, #2790 ) ;
#2334 = ORIENTED_EDGE ( 'NONE', *, *, #391, .T. ) ;
#2335 = SURFACE_SIDE_STYLE ('',( #5281 ) ) ;
#2336 = ORIENTED_EDGE ( 'NONE', *, *, #535, .T. ) ;
#2337 = VECTOR ( 'NONE', #3898, 1000.000000000000000 ) ;
#2338 = EDGE_CURVE ( 'NONE', #2607, #3420, #1443, .T. ) ;
#2339 = AXIS2_PLACEMENT_3D ( 'NONE', #806, #1378, #497 ) ;
#2340 = ORIENTED_EDGE ( 'NONE', *, *, #3767, .F. ) ;
#2341 = EDGE_CURVE ( 'NONE', #2368, #1732, #3459, .T. ) ;
#2342 = ORIENTED_EDGE ( 'NONE', *, *, #4716, .F. ) ;
#2343 = LINE ( 'NONE', #677, #3085 ) ;
#2344 = FACE_BOUND ( 'NONE', #33, .T. ) ;
#2345 = ORIENTED_EDGE ( 'NONE', *, *, #1169, .F. ) ;
#2346 = ORIENTED_EDGE ( 'NONE', *, *, #211, .T. ) ;
#2347 = CARTESIAN_POINT ( 'NONE',  ( -9.000000000000000000, 5.196152422706629359, -8.935996291721334472 ) ) ;
#2348 = CARTESIAN_POINT ( 'NONE',  ( -2.893723230124264134, -8.721612959540728127, -9.019248292998303995 ) ) ;
#2349 = CARTESIAN_POINT ( 'NONE',  ( 0.000000000000000000, 10.39230484541326760, -1.199999999999999734 ) ) ;
#2350 = LINE ( 'NONE', #1927, #154 ) ;
#2351 = DIRECTION ( 'NONE',  ( 0.000000000000000000, 0.000000000000000000, 1.000000000000000000 ) ) ;
#2352 = ORIENTED_EDGE ( 'NONE', *, *, #762, .F. ) ;
#2353 = ORIENTED_EDGE ( 'NONE', *, *, #136, .F. ) ;
#2354 = CARTESIAN_POINT ( 'NONE',  ( -25.00000000000000000, 10.00000000000000000, 25.00000000000000000 ) ) ;
#2355 = VERTEX_POINT ( 'NONE', #1530 ) ;
#2356 = DIRECTION ( 'NONE',  ( 0.000000000000000000, 0.000000000000000000, -1.000000000000000000 ) ) ;
#2357 = CARTESIAN_POINT ( 'NONE',  ( 137.5000000000000000, 870.0000000000000000, 0.000000000000000000 ) ) ;
#2358 = CARTESIAN_POINT ( 'NONE',  ( 0.000000000000000000, -10.39230484541327293, -8.935996291721338025 ) ) ;
#2359 =( BOUNDED_SURFACE ( )  B_SPLINE_SURFACE ( 3, 2, ( 
 ( #476, #113, #2165 ),
 ( #1730, #94, #4267 ),
 ( #1367, #5033, #3349 ),
 ( #3407, #1672, #3835 ),
 ( #5081, #865, #1337 ),
 ( #1753, #2192, #2084 ),
 ( #527, #1295, #2104 ),
 ( #2532, #446, #5110 ) ),
 .UNSPECIFIED., .F., .F., .F. ) 
 B_SPLINE_SURFACE_WITH_KNOTS ( ( 4, 2, 2, 4 ),
 ( 3, 3 ),
 ( 0.04613854442509285336, 0.05169925677048779755, 0.05447961294318526965, 0.05725996911588274174 ),
 ( 0.000000000000000000, 1.000000000000000000 ),
 .UNSPECIFIED. ) 
 GEOMETRIC_REPRESENTATION_ITEM ( )  RATIONAL_B_SPLINE_SURFACE ( (
 ( 1.000000000000000000, 0.8047781684971936356, 1.000000000000000000),
 ( 1.000000000000000000, 0.8123765127741280345, 1.000000000000000000),
 ( 1.000000000000000000, 0.8190661184402779904, 1.000000000000000000),
 ( 1.000000000000000000, 0.8191936944251213548, 1.000000000000000000),
 ( 1.000000000000000000, 0.8176092056339585579, 1.000000000000000000),
 ( 1.000000000000000000, 0.8122961334886904528, 1.000000000000000000),
 ( 1.000000000000000000, 0.8086310951057497087, 1.000000000000000000),
 ( 1.000000000000000000, 0.8047712311394934481, 1.000000000000000000) ) ) 
 REPRESENTATION_ITEM ( '' )  SURFACE ( )  );
#2360 = CARTESIAN_POINT ( 'NONE',  ( 137.5000000000000000, 870.0000000000000000, -20.00000000000001421 ) ) ;
#2361 = FACE_OUTER_BOUND ( 'NONE', #3559, .T. ) ;
#2362 = EDGE_LOOP ( 'NONE', ( #974, #2920 ) ) ;
#2363 =( NAMED_UNIT ( * ) SI_UNIT ( $, .STERADIAN. ) SOLID_ANGLE_UNIT ( ) );
#2364 = CIRCLE ( 'NONE', #2804, 15.00000000000000000 ) ;
#2365 = VERTEX_POINT ( 'NONE', #1516 ) ;
#2366 = SURFACE_SIDE_STYLE ('',( #2008 ) ) ;
#2367 = SURFACE_STYLE_FILL_AREA ( #4040 ) ;
#2368 = VERTEX_POINT ( 'NONE', #1558 ) ;
#2369 = CARTESIAN_POINT ( 'NONE',  ( 6.499999999999988454, 510.0000000000000000, 25.00000000000000000 ) ) ;
#2370 = ADVANCED_FACE ( 'NONE', ( #2864 ), #4509, .T. ) ;
#2371 = ORIENTED_EDGE ( 'NONE', *, *, #3216, .F. ) ;
#2372 = VERTEX_POINT ( 'NONE', #3326 ) ;
#2373 = DIRECTION ( 'NONE',  ( -0.000000000000000000, -0.000000000000000000, 1.000000000000000000 ) ) ;
#2374 = CARTESIAN_POINT ( 'NONE',  ( 0.3349232592648707096, -10.58567287930771350, -9.544071379897779650 ) ) ;
#2375 = PLANE ( 'NONE',  #2861 ) ;
#2376 = DIRECTION ( 'NONE',  ( -0.000000000000000000, -0.000000000000000000, 1.000000000000000000 ) ) ;
#2377 = UNCERTAINTY_MEASURE_WITH_UNIT (LENGTH_MEASURE( 1.000000000000000082E-05 ), #1538, 'distance_accuracy_value', 'NONE');
#2378 = APPLICATION_PROTOCOL_DEFINITION ( 'draft international standard', 'automotive_design', 1998, #501 ) ;
#2379 = ORIENTED_EDGE ( 'NONE', *, *, #1755, .T. ) ;
#2380 = ORIENTED_EDGE ( 'NONE', *, *, #4566, .F. ) ;
#2381 = LINE ( 'NONE', #2443, #4305 ) ;
#2382 = VERTEX_POINT ( 'NONE', #1646 ) ;
#2383 = CARTESIAN_POINT ( 'NONE',  ( 0.000000000000000000, 450.0000000000000000, 25.00000000000000000 ) ) ;
#2384 = FACE_OUTER_BOUND ( 'NONE', #1627, .T. ) ;
#2385 = DIRECTION ( 'NONE',  ( 1.000000000000000000, 0.000000000000000000, 0.000000000000000000 ) ) ;
#2386 = LINE ( 'NONE', #280, #2074 ) ;
#2387 = EDGE_CURVE ( 'NONE', #1591, #2639, #4557, .T. ) ;
#2388 = CIRCLE ( 'NONE', #2564, 6.000000000000000000 ) ;
#2389 = DIRECTION ( 'NONE',  ( 0.000000000000000000, 0.000000000000000000, 1.000000000000000000 ) ) ;
#2390 = CARTESIAN_POINT ( 'NONE',  ( 0.000000000000000000, 210.0000000000000284, 0.000000000000000000 ) ) ;
#2391 = ADVANCED_FACE ( 'NONE', ( #3620 ), #2899, .F. ) ;
#2392 = ORIENTED_EDGE ( 'NONE', *, *, #2151, .T. ) ;
#2393 =( LENGTH_UNIT ( ) NAMED_UNIT ( * ) SI_UNIT ( .MILLI., .METRE. ) );
#2394 = VERTEX_POINT ( 'NONE', #2505 ) ;
#2395 = CIRCLE ( 'NONE', #3619, 9.000000000000001776 ) ;
#2396 = ORIENTED_EDGE ( 'NONE', *, *, #3766, .F. ) ;
#2397 = VECTOR ( 'NONE', #1738, 1000.000000000000227 ) ;
#2398 = DIRECTION ( 'NONE',  ( 5.551115123125753120E-16, 1.000000000000000000, 1.155557966632335381E-31 ) ) ;
#2399 = CYLINDRICAL_SURFACE ( 'NONE', #744, 6.499999999999988454 ) ;
#2400 = EDGE_LOOP ( 'NONE', ( #5036, #4952, #2889, #5202, #1404 ) ) ;
#2401 = ADVANCED_FACE ( 'NONE', ( #3236 ), #3683, .F. ) ;
#2402 = CARTESIAN_POINT ( 'NONE',  ( 9.506737344437272696, -5.488717364925930653, -9.686084310752812954 ) ) ;
#2403 = AXIS2_PLACEMENT_3D ( 'NONE', #4485, #5343, #766 ) ;
#2404 = VERTEX_POINT ( 'NONE', #2425 ) ;
#2405 = CARTESIAN_POINT ( 'NONE',  ( 0.000000000000000000, 0.000000000000000000, -25.00000000000000000 ) ) ;
#2406 = CARTESIAN_POINT ( 'NONE',  ( 150.0000000000000000, 10.00000000000000000, -150.0000000000000000 ) ) ;
#2407 = DIRECTION ( 'NONE',  ( 0.000000000000000000, 0.000000000000000000, -1.000000000000000000 ) ) ;
#2408 = FACE_OUTER_BOUND ( 'NONE', #3454, .T. ) ;
#2409 = PRODUCT_DEFINITION_SHAPE ( 'NONE', 'NONE',  #182 ) ;
#2410 =( LENGTH_UNIT ( ) NAMED_UNIT ( * ) SI_UNIT ( .MILLI., .METRE. ) );
#2411 = PRESENTATION_LAYER_ASSIGNMENT (  '', '', ( #4732 ) ) ;
#2412 = AXIS2_PLACEMENT_3D ( 'NONE', #5221, #4798, #3535 ) ;
#2413 = ORIENTED_EDGE ( 'NONE', *, *, #5071, .F. ) ;
#2414 = EDGE_CURVE ( 'NONE', #4789, #4512, #834, .T. ) ;
#2415 = PLANE ( 'NONE',  #5008 ) ;
#2416 = ORIENTED_EDGE ( 'NONE', *, *, #4972, .F. ) ;
#2417 = CARTESIAN_POINT ( 'NONE',  ( -1.899904140753538487E-15, -10.46021122251003277, -9.269271692759762260 ) ) ;
#2418 = FACE_BOUND ( 'NONE', #5367, .T. ) ;
#2419 = ADVANCED_FACE ( 'NONE', ( #344 ), #1132, .T. ) ;
#2420 = CARTESIAN_POINT ( 'NONE',  ( 0.7810345657019077681, 10.51638858288773015, -9.518277236634762772 ) ) ;
#2421 = CIRCLE ( 'NONE', #847, 6.499999999999983125 ) ;
#2422 = VECTOR ( 'NONE', #3914, 1000.000000000000114 ) ;
#2423 = VECTOR ( 'NONE', #1924, 1000.000000000000000 ) ;
#2424 = ORIENTED_EDGE ( 'NONE', *, *, #473, .T. ) ;
#2425 = CARTESIAN_POINT ( 'NONE',  ( 6.499999999999981348, 35.00000000000000000, 25.00000000000000000 ) ) ;
#2426 = CYLINDRICAL_SURFACE ( 'NONE', #420, 15.00000000000000000 ) ;
#2427 = EDGE_LOOP ( 'NONE', ( #3156, #4006 ) ) ;
#2428 = SHAPE_REPRESENTATION_RELATIONSHIP ( 'NONE' , 'NONE' ,  #3863, #387 ) ;
#2429 = VECTOR ( 'NONE', #959, 1000.000000000000000 ) ;
#2430 = VECTOR ( 'NONE', #1381, 1000.000000000000000 ) ;
#2431 = FACE_OUTER_BOUND ( 'NONE', #4868, .T. ) ;
#2432 = CARTESIAN_POINT ( 'NONE',  ( -139.9999999999999716, 885.0000000000000000, 25.00000000000000000 ) ) ;
#2433 = EDGE_LOOP ( 'NONE', ( #1007, #3544, #2793, #1157 ) ) ;
#2434 = CARTESIAN_POINT ( 'NONE',  ( 0.000000000000000000, 0.000000000000000000, 0.000000000000000000 ) ) ;
#2435 = VECTOR ( 'NONE', #2620, 1000.000000000000000 ) ;
#2436 = CIRCLE ( 'NONE', #3125, 9.000000000000001776 ) ;
#2437 = ADVANCED_FACE ( 'NONE', ( #3660 ), #1242, .F. ) ;
#2438 = VERTEX_POINT ( 'NONE', #393 ) ;
#2439 = CARTESIAN_POINT ( 'NONE',  ( -121.7157287525381122, 0.000000000000000000, 121.7157287525380127 ) ) ;
#2440 = DIRECTION ( 'NONE',  ( -0.000000000000000000, -1.000000000000000000, -0.000000000000000000 ) ) ;
#2441 = CARTESIAN_POINT ( 'NONE',  ( 9.506737344437272696, 5.488717364925924436, -9.686084310752812954 ) ) ;
#2442 = DIRECTION ( 'NONE',  ( 0.000000000000000000, 0.000000000000000000, 1.000000000000000000 ) ) ;
#2443 = CARTESIAN_POINT ( 'NONE',  ( 7.347880794884117764E-16, 810.0000000000000000, 5.999999999999998224 ) ) ;
#2444 = ORIENTED_EDGE ( 'NONE', *, *, #206, .F. ) ;
#2445 = DIRECTION ( 'NONE',  ( -0.000000000000000000, -1.000000000000000000, -0.000000000000000000 ) ) ;
#2446 = PLANE ( 'NONE',  #5377 ) ;
#2447 = FACE_OUTER_BOUND ( 'NONE', #324, .T. ) ;
#2448 = CARTESIAN_POINT ( 'NONE',  ( 6.329281523778166552, 7.289348427314501500, -9.189707035345829667 ) ) ;
#2449 = EDGE_CURVE ( 'NONE', #428, #3262, #811, .T. ) ;
#2450 = CARTESIAN_POINT ( 'NONE',  ( -1.676835913137321903E-15, 35.00000000000000000, 30.00000000000000711 ) ) ;
#2451 = CARTESIAN_POINT ( 'NONE',  ( -1.500000000000000444, 9.526279441628826561, -8.667800885990208926 ) ) ;
#2452 = ORIENTED_EDGE ( 'NONE', *, *, #2562, .T. ) ;
#2453 = ORIENTED_EDGE ( 'NONE', *, *, #3245, .F. ) ;
#2454 = VERTEX_POINT ( 'NONE', #5279 ) ;
#2455 = CARTESIAN_POINT ( 'NONE',  ( -150.0000000000000000, 885.0000000000000000, 25.00000000000000000 ) ) ;
#2456 = ORIENTED_EDGE ( 'NONE', *, *, #1341, .T. ) ;
#2457 = FILL_AREA_STYLE ('',( #3334 ) ) ;
#2458 = APPLICATION_CONTEXT ( 'automotive_design' ) ;
#2459 = EDGE_LOOP ( 'NONE', ( #512, #3271, #888, #4241 ) ) ;
#2460 = ADVANCED_FACE ( 'NONE', ( #1158 ), #367, .F. ) ;
#2461 = EDGE_LOOP ( 'NONE', ( #1801, #2012, #3367, #4779 ) ) ;
#2462 = DIRECTION ( 'NONE',  ( 0.000000000000000000, -1.224646799147353207E-16, 1.000000000000000000 ) ) ;
#2463 = CARTESIAN_POINT ( 'NONE',  ( 0.4165158504820782315, 10.63278038381083945, -9.021433408186453562 ) ) ;
#2464 = CARTESIAN_POINT ( 'NONE',  ( 0.000000000000000000, 0.000000000000000000, 0.000000000000000000 ) ) ;
#2465 = CARTESIAN_POINT ( 'NONE',  ( 2.790577774332637429, -8.781164016207737788, -8.465119797811231805 ) ) ;
#2466 = SHAPE_DEFINITION_REPRESENTATION ( #5021, #1620 ) ;
#2467 = EDGE_CURVE ( 'NONE', #3611, #5063, #1865, .T. ) ;
#2468 = CARTESIAN_POINT ( 'NONE',  ( 6.000000000000000000, 0.000000000000000000, 0.000000000000000000 ) ) ;
#2469 = DIRECTION ( 'NONE',  ( 1.000000000000000000, 0.000000000000000000, 0.000000000000000000 ) ) ;
#2470 = SURFACE_SIDE_STYLE ('',( #897 ) ) ;
#2471 = DIRECTION ( 'NONE',  ( 0.000000000000000000, 0.000000000000000000, 1.000000000000000000 ) ) ;
#2472 = CARTESIAN_POINT ( 'NONE',  ( 7.923304691439484237, 6.383148552592245117, -9.380055053747694771 ) ) ;
#2473 = EDGE_CURVE ( 'NONE', #3402, #273, #1270, .T. ) ;
#2474 = ORIENTED_EDGE ( 'NONE', *, *, #1651, .T. ) ;
#2475 = CARTESIAN_POINT ( 'NONE',  ( 0.000000000000000000, 450.0000000000000000, 25.00000000000000000 ) ) ;
#2476 = DIRECTION ( 'NONE',  ( -0.000000000000000000, -0.000000000000000000, 1.000000000000000000 ) ) ;
#2477 = ORIENTED_EDGE ( 'NONE', *, *, #728, .F. ) ;
#2478 = VERTEX_POINT ( 'NONE', #5337 ) ;
#2479 = ORIENTED_EDGE ( 'NONE', *, *, #2160, .F. ) ;
#2480 = LINE ( 'NONE', #2512, #3721 ) ;
#2481 = EDGE_CURVE ( 'NONE', #2146, #5319, #1609, .T. ) ;
#2482 = VECTOR ( 'NONE', #3550, 1000.000000000000000 ) ;
#2483 = ORIENTED_EDGE ( 'NONE', *, *, #11, .F. ) ;
#2484 = SHAPE_REPRESENTATION_RELATIONSHIP ( 'NONE' , 'NONE' ,  #3706, #2946 ) ;
#2485 = EDGE_CURVE ( 'NONE', #656, #701, #4587, .T. ) ;
#2486 = CIRCLE ( 'NONE', #2119, 5.999999999999993783 ) ;
#2487 = ORIENTED_EDGE ( 'NONE', *, *, #4218, .T. ) ;
#2488 = DIRECTION ( 'NONE',  ( 1.000000000000000000, 0.000000000000000000, 0.000000000000000000 ) ) ;
#2489 = FACE_OUTER_BOUND ( 'NONE', #5079, .T. ) ;
#2490 = CARTESIAN_POINT ( 'NONE',  ( -150.0000000000000000, 885.0000000000000000, 25.00000000000000000 ) ) ;
#2491 = FACE_OUTER_BOUND ( 'NONE', #45, .T. ) ;
#2492 = CONICAL_SURFACE ( 'NONE', #3525, 5.057500000000000107, 1.047197551196592302 ) ;
#2493 = ADVANCED_FACE ( 'NONE', ( #3761 ), #4611, .F. ) ;
#2494 = AXIS2_PLACEMENT_3D ( 'NONE', #1451, #3153, #1055 ) ;
#2495 = ORIENTED_EDGE ( 'NONE', *, *, #4972, .T. ) ;
#2496 = CARTESIAN_POINT ( 'NONE',  ( 91.03600000000004400, 0.000000000000000000, 0.000000000000000000 ) ) ;
#2497 = DIRECTION ( 'NONE',  ( 6.938893903907228378E-17, 0.000000000000000000, -1.000000000000000000 ) ) ;
#2498 = CARTESIAN_POINT ( 'NONE',  ( -6.499999999999984901, 35.00000000000000000, -25.00000000000000000 ) ) ;
#2499 = CARTESIAN_POINT ( 'NONE',  ( -9.473648099969723901, -0.9041442221342959051, -9.137386922016339952 ) ) ;
#2500 = AXIS2_PLACEMENT_3D ( 'NONE', #2716, #3940, #224 ) ;
#2501 = COLOUR_RGB ( '',0.8941176470588234615, 0.8941176470588234615, 0.8941176470588234615 ) ;
#2502 = ADVANCED_FACE ( 'NONE', ( #3381 ), #2134, .T. ) ;
#2503 = TOROIDAL_SURFACE ( 'NONE', #3806, 12.07201791628681598, 0.9279820837131842470 ) ;
#2504 = ORIENTED_EDGE ( 'NONE', *, *, #1202, .F. ) ;
#2505 = CARTESIAN_POINT ( 'NONE',  ( -6.499999999999988454, 570.0000000000000000, 25.00000000000000000 ) ) ;
#2506 = UNCERTAINTY_MEASURE_WITH_UNIT (LENGTH_MEASURE( 1.000000000000000082E-05 ), #431, 'distance_accuracy_value', 'NONE');
#2507 = CARTESIAN_POINT ( 'NONE',  ( 0.7813822207450755730, -10.51618336147352295, -9.518202542148555878 ) ) ;
#2508 = ORIENTED_EDGE ( 'NONE', *, *, #737, .T. ) ;
#2509 = VERTEX_POINT ( 'NONE', #21 ) ;
#2510 = ORIENTED_EDGE ( 'NONE', *, *, #3208, .F. ) ;
#2511 = AXIS2_PLACEMENT_3D ( 'NONE', #3251, #2015, #3226 ) ;
#2512 = CARTESIAN_POINT ( 'NONE',  ( -25.00000000000000000, 10.00000000000000000, 24.99999999999999645 ) ) ;
#2513 = ORIENTED_EDGE ( 'NONE', *, *, #3038, .F. ) ;
#2514 = EDGE_LOOP ( 'NONE', ( #360, #2646, #1877, #1293 ) ) ;
#2515 = AXIS2_PLACEMENT_3D ( 'NONE', #1485, #4106, #5296 ) ;
#2516 = ADVANCED_FACE ( 'NONE', ( #3043 ), #2359, .F. ) ;
#2517 = B_SPLINE_CURVE_WITH_KNOTS ( 'NONE', 3,
 ( #4000, #626, #250, #1879, #168, #980, #3883, #2655 ),
 .UNSPECIFIED., .F., .F.,
 ( 4, 2, 2, 4 ),
 ( 0.007274027330054943195, 0.008608952725826013452, 0.009943878121597081107, 0.01261372891313921468 ),
 .UNSPECIFIED. ) ;
#2518 = EDGE_CURVE ( 'NONE', #1856, #2978, #4073, .T. ) ;
#2519 = ORIENTED_EDGE ( 'NONE', *, *, #4887, .T. ) ;
#2520 = CARTESIAN_POINT ( 'NONE',  ( 12.59999999999999964, 8.082668874372532992E-16, 6.600000000000001421 ) ) ;
#2521 = LINE ( 'NONE', #2116, #325 ) ;
#2522 = CARTESIAN_POINT ( 'NONE',  ( -9.000000000000001776, -4.785828667975444262, -1.023175036954117711 ) ) ;
#2523 = AXIS2_PLACEMENT_3D ( 'NONE', #1360, #4386, #2263 ) ;
#2524 = B_SPLINE_CURVE_WITH_KNOTS ( 'NONE', 3,
 ( #1183, #2825, #4506, #3234, #3171, #4824, #4032, #697, #2358 ),
 .UNSPECIFIED., .F., .F.,
 ( 4, 2, 1, 2, 4 ),
 ( 0.000000000000000000, 0.002598076211353316737, 0.005196152422706633474, 0.007794228634059948910, 0.01039230484541326521 ),
 .UNSPECIFIED. ) ;
#2525 = DIRECTION ( 'NONE',  ( 0.000000000000000000, 1.000000000000000000, 0.000000000000000000 ) ) ;
#2526 = CARTESIAN_POINT ( 'NONE',  ( -1.301042606982605321E-14, -10.39230484541326760, -1.199999999999999734 ) ) ;
#2527 = CARTESIAN_POINT ( 'NONE',  ( -2.951638237467835602, 8.688175714460818710, -0.1192015822679155373 ) ) ;
#2528 = CARTESIAN_POINT ( 'NONE',  ( -9.498409640465782289, -4.629036869500566809, -9.525571706933844141 ) ) ;
#2529 = VERTEX_POINT ( 'NONE', #3428 ) ;
#2530 = DIRECTION ( 'NONE',  ( 0.000000000000000000, 0.000000000000000000, -1.000000000000000000 ) ) ;
#2531 = ADVANCED_FACE ( 'NONE', ( #2585 ), #1774, .F. ) ;
#2532 = CARTESIAN_POINT ( 'NONE',  ( -0.4179773697347383132, 10.63362419234479006, -9.021743230619932774 ) ) ;
#2533 = CARTESIAN_POINT ( 'NONE',  ( 6.000000000000000000, -5.839897972853064445, 4.770489558936219510E-15 ) ) ;
#2534 = VERTEX_POINT ( 'NONE', #957 ) ;
#2535 = ORIENTED_EDGE ( 'NONE', *, *, #2705, .T. ) ;
#2536 = PRODUCT_DEFINITION ( 'UNKNOWN', '', #4228, #4292 ) ;
#2537 = CARTESIAN_POINT ( 'NONE',  ( -121.7157287525392917, -20.00000000000000000, -136.7157287525368474 ) ) ;
#2538 = ORIENTED_EDGE ( 'NONE', *, *, #1792, .T. ) ;
#2539 = VERTEX_POINT ( 'NONE', #4244 ) ;
#2540 = EDGE_LOOP ( 'NONE', ( #4104, #5, #404, #4888, #4096 ) ) ;
#2541 =( BOUNDED_SURFACE ( )  B_SPLINE_SURFACE ( 3, 2, ( 
 ( #606, #4830, #3127 ),
 ( #1935, #3094, #4370 ),
 ( #230, #1470, #3945 ),
 ( #633, #2301, #666 ),
 ( #4033, #1886, #4771 ),
 ( #1050, #256, #5141 ),
 ( #2718, #2744, #4008 ),
 ( #4350, #175, #3070 ) ),
 .UNSPECIFIED., .F., .F., .F. ) 
 B_SPLINE_SURFACE_WITH_KNOTS ( ( 4, 2, 2, 4 ),
 ( 3, 3 ),
 ( 0.04599591305096960986, 0.05155656099146234406, 0.05433688496170870769, 0.05711720893195507132 ),
 ( 0.000000000000000000, 1.000000000000000000 ),
 .UNSPECIFIED. ) 
 GEOMETRIC_REPRESENTATION_ITEM ( )  RATIONAL_B_SPLINE_SURFACE ( (
 ( 1.000000000000000000, 0.8047781771973553377, 1.000000000000000000),
 ( 1.000000000000000000, 0.8123762916867537376, 1.000000000000000000),
 ( 1.000000000000000000, 0.8190655187926852987, 1.000000000000000000),
 ( 1.000000000000000000, 0.8191939758637984959, 1.000000000000000000),
 ( 1.000000000000000000, 0.8176095670996671450, 1.000000000000000000),
 ( 1.000000000000000000, 0.8122963966407920067, 1.000000000000000000),
 ( 1.000000000000000000, 0.8086312082325360917, 1.000000000000000000),
 ( 1.000000000000000000, 0.8047712221770487728, 1.000000000000000000) ) ) 
 REPRESENTATION_ITEM ( '' )  SURFACE ( )  );
#2542 = CARTESIAN_POINT ( 'NONE',  ( 0.000000000000000000, 0.000000000000000000, 0.000000000000000000 ) ) ;
#2543 = EDGE_CURVE ( 'NONE', #2607, #2534, #5001, .T. ) ;
#2544 = CARTESIAN_POINT ( 'NONE',  ( 0.3334815747005966946, 10.58484052233643524, -9.543752552345290852 ) ) ;
#2545 = CARTESIAN_POINT ( 'NONE',  ( 137.5000000000000000, 870.0000000000000000, 0.000000000000000000 ) ) ;
#2546 = EDGE_LOOP ( 'NONE', ( #3922, #3951, #2593, #151 ) ) ;
#2547 = CIRCLE ( 'NONE', #3000, 6.499999999999988454 ) ;
#2548 = DIRECTION ( 'NONE',  ( 1.000000000000000000, 0.000000000000000000, 0.000000000000000000 ) ) ;
#2549 = ORIENTED_EDGE ( 'NONE', *, *, #1193, .F. ) ;
#2550 = CARTESIAN_POINT ( 'NONE',  ( -6.245004513516506329E-15, 557.4999999999997726, 50.00000000000000000 ) ) ;
#2551 = LINE ( 'NONE', #63, #2145 ) ;
#2552 = CIRCLE ( 'NONE', #2988, 5.999999999999950262 ) ;
#2553 = CARTESIAN_POINT ( 'NONE',  ( 137.5000000000000000, 870.0000000000000000, -6.000000000000006217 ) ) ;
#2554 = CARTESIAN_POINT ( 'NONE',  ( 7.500000000000000000, -6.062177826491074839, -8.667800885990210702 ) ) ;
#2555 =( NAMED_UNIT ( * ) PLANE_ANGLE_UNIT ( ) SI_UNIT ( $, .RADIAN. ) );
#2556 = VERTEX_POINT ( 'NONE', #884 ) ;
#2557 = ORIENTED_EDGE ( 'NONE', *, *, #69, .T. ) ;
#2558 = CARTESIAN_POINT ( 'NONE',  ( 0.000000000000000000, 810.0000000000000000, 0.000000000000000000 ) ) ;
#2559 = DIRECTION ( 'NONE',  ( -0.000000000000000000, -0.000000000000000000, -1.000000000000000000 ) ) ;
#2560 = ORIENTED_EDGE ( 'NONE', *, *, #3359, .T. ) ;
#2561 = EDGE_CURVE ( 'NONE', #2324, #4507, #2221, .T. ) ;
#2562 = EDGE_CURVE ( 'NONE', #3895, #457, #1707, .T. ) ;
#2563 = LINE ( 'NONE', #1342, #3179 ) ;
#2564 = AXIS2_PLACEMENT_3D ( 'NONE', #4336, #2373, #4438 ) ;
#2565 = ORIENTED_EDGE ( 'NONE', *, *, #3260, .F. ) ;
#2566 = EDGE_CURVE ( 'NONE', #4832, #4261, #4291, .T. ) ;
#2567 = PLANE ( 'NONE',  #4064 ) ;
#2568 = CARTESIAN_POINT ( 'NONE',  ( 121.7157287525384533, -20.00000000000000000, 121.7157287525376859 ) ) ;
#2569 = CARTESIAN_POINT ( 'NONE',  ( -1.219033264612565448, 9.688495661947332138, -9.200452032552545845 ) ) ;
#2570 = CARTESIAN_POINT ( 'NONE',  ( 0.000000000000000000, 0.000000000000000000, -25.03750572909317285 ) ) ;
#2571 = AXIS2_PLACEMENT_3D ( 'NONE', #2201, #3775, #2120 ) ;
#2572 = CARTESIAN_POINT ( 'NONE',  ( -137.5000000000000000, 870.0000000000000000, 0.000000000000000000 ) ) ;
#2573 = AXIS2_PLACEMENT_3D ( 'NONE', #3101, #4431, #3630 ) ;
#2574 = CARTESIAN_POINT ( 'NONE',  ( 0.000000000000000000, 570.0000000000000000, 25.00000000000000000 ) ) ;
#2575 = LINE ( 'NONE', #4281, #5197 ) ;
#2576 = CARTESIAN_POINT ( 'NONE',  ( 0.000000000000000000, 10.39230484541326760, -1.199999999999999734 ) ) ;
#2577 = CARTESIAN_POINT ( 'NONE',  ( 6.000000000000000000, 2.919948986426526005, -5.057500000000002771 ) ) ;
#2578 = SURFACE_SIDE_STYLE ('',( #68 ) ) ;
#2579 = CIRCLE ( 'NONE', #4148, 0.5999999999999998668 ) ;
#2580 = ADVANCED_FACE ( 'NONE', ( #2692 ), #4738, .T. ) ;
#2581 = ADVANCED_FACE ( 'NONE', ( #1830 ), #2270, .F. ) ;
#2582 = ORIENTED_EDGE ( 'NONE', *, *, #433, .T. ) ;
#2583 = CARTESIAN_POINT ( 'NONE',  ( 6.000000000000000000, -2.919948986426526893, 5.057500000000001883 ) ) ;
#2584 = CARTESIAN_POINT ( 'NONE',  ( 0.000000000000000000, 0.000000000000000000, -11.97459999999999880 ) ) ;
#2585 = FACE_OUTER_BOUND ( 'NONE', #1937, .T. ) ;
#2586 = DIRECTION ( 'NONE',  ( -0.000000000000000000, 0.000000000000000000, 1.000000000000000000 ) ) ;
#2587 = AXIS2_PLACEMENT_3D ( 'NONE', #2558, #4211, #2632 ) ;
#2588 = ORIENTED_EDGE ( 'NONE', *, *, #1021, .T. ) ;
#2589 = PRODUCT_DEFINITION_SHAPE ( 'NONE', 'NONE',  #2188 ) ;
#2590 = DIRECTION ( 'NONE',  ( 1.000000000000000000, 0.000000000000000000, 0.000000000000000000 ) ) ;
#2591 = AXIS2_PLACEMENT_3D ( 'NONE', #2289, #949, #1902 ) ;
#2592 = AXIS2_PLACEMENT_3D ( 'NONE', #1232, #5380, #4932 ) ;
#2593 = ORIENTED_EDGE ( 'NONE', *, *, #4981, .T. ) ;
#2594 = CARTESIAN_POINT ( 'NONE',  ( -1.676835913137321903E-15, 35.00000000000000000, 30.00000000000000711 ) ) ;
#2595 = CARTESIAN_POINT ( 'NONE',  ( -150.0000000000000284, 10.00000000000000000, -150.0000000000000853 ) ) ;
#2596 = DIRECTION ( 'NONE',  ( 1.000000000000000000, 0.000000000000000000, 0.000000000000000000 ) ) ;
#2597 = CONTEXT_DEPENDENT_SHAPE_REPRESENTATION ( #3995, #3935 ) ;
#2598 = AXIS2_PLACEMENT_3D ( 'NONE', #2496, #4111, #3755 ) ;
#2599 = AXIS2_PLACEMENT_3D ( 'NONE', #1497, #4686, #3069 ) ;
#2600 = PRODUCT_RELATED_PRODUCT_CATEGORY ( 'part', '', ( #4971 ) ) ;
#2601 =( REPRESENTATION_RELATIONSHIP ('NONE','NONE', #4791, #121 ) REPRESENTATION_RELATIONSHIP_WITH_TRANSFORMATION ( #3754 )SHAPE_REPRESENTATION_RELATIONSHIP( ) );
#2602 = CARTESIAN_POINT ( 'NONE',  ( -30.00000000000000000, 10.00000000000000000, -30.00000000000000355 ) ) ;
#2603 = CARTESIAN_POINT ( 'NONE',  ( -1.676835913137321903E-15, 35.00000000000000000, 30.00000000000000711 ) ) ;
#2604 = FACE_OUTER_BOUND ( 'NONE', #1189, .T. ) ;
#2605 = AXIS2_PLACEMENT_3D ( 'NONE', #4464, #5350, #4414 ) ;
#2606 = CARTESIAN_POINT ( 'NONE',  ( -1.676835913137321903E-15, 35.00000000000000000, 25.00000000000000000 ) ) ;
#2607 = VERTEX_POINT ( 'NONE', #3590 ) ;
#2608 = DIRECTION ( 'NONE',  ( -0.000000000000000000, 0.000000000000000000, -1.000000000000000000 ) ) ;
#2609 = AXIS2_PLACEMENT_3D ( 'NONE', #4275, #3492, #2596 ) ;
#2610 = ORIENTED_EDGE ( 'NONE', *, *, #4201, .T. ) ;
#2611 = DIRECTION ( 'NONE',  ( -1.000000000000000000, 0.000000000000000000, 0.000000000000000000 ) ) ;
#2612 = DIRECTION ( 'NONE',  ( -0.000000000000000000, 0.000000000000000000, 1.000000000000000000 ) ) ;
#2613 = EDGE_CURVE ( 'NONE', #432, #4946, #2216, .T. ) ;
#2614 = DIRECTION ( 'NONE',  ( -1.000000000000000000, -0.000000000000000000, -0.000000000000000000 ) ) ;
#2615 =( LENGTH_UNIT ( ) NAMED_UNIT ( * ) SI_UNIT ( .MILLI., .METRE. ) );
#2616 = ORIENTED_EDGE ( 'NONE', *, *, #4297, .T. ) ;
#2617 = B_SPLINE_CURVE_WITH_KNOTS ( 'NONE', 3,
 ( #2526, #4204, #440, #1309, #5026, #1287, #2966, #2124 ),
 .UNSPECIFIED., .F., .F.,
 ( 4, 2, 2, 4 ),
 ( 2.475501737064928787E-07, 0.002666746755945506933, 0.003999996358831405148, 0.005333245961717304230 ),
 .UNSPECIFIED. ) ;
#2618 = EDGE_LOOP ( 'NONE', ( #4569, #4690, #424, #3356 ) ) ;
#2619 = PLANE ( 'NONE',  #3434 ) ;
#2620 = DIRECTION ( 'NONE',  ( -1.000000000000000000, -0.000000000000000000, -0.000000000000000000 ) ) ;
#2621 = EDGE_CURVE ( 'NONE', #4335, #1561, #129, .T. ) ;
#2622 = CARTESIAN_POINT ( 'NONE',  ( -9.000000000000001776, 0.2246546977803019485, 1.534188425714351489E-15 ) ) ;
#2623 = CARTESIAN_POINT ( 'NONE',  ( 9.000000000000001776, 0.000000000000000000, 0.000000000000000000 ) ) ;
#2624 = EDGE_CURVE ( 'NONE', #2728, #4553, #750, .T. ) ;
#2625 = CYLINDRICAL_SURFACE ( 'NONE', #228, 6.000000000000000888 ) ;
#2626 = PLANE ( 'NONE',  #3396 ) ;
#2627 = VECTOR ( 'NONE', #170, 999.9999999999998863 ) ;
#2628 = LINE ( 'NONE', #1067, #1777 ) ;
#2629 = ORIENTED_EDGE ( 'NONE', *, *, #3048, .F. ) ;
#2630 = LINE ( 'NONE', #72, #1053 ) ;
#2631 = CARTESIAN_POINT ( 'NONE',  ( 25.00000000000000000, 810.0000000000000000, -25.00000000000000000 ) ) ;
#2632 = DIRECTION ( 'NONE',  ( 0.000000000000000000, 0.000000000000000000, 1.000000000000000000 ) ) ;
#2633 = FACE_OUTER_BOUND ( 'NONE', #1391, .T. ) ;
#2634 = ORIENTED_EDGE ( 'NONE', *, *, #1896, .T. ) ;
#2635 = DIRECTION ( 'NONE',  ( 0.000000000000000000, 0.000000000000000000, 1.000000000000000000 ) ) ;
#2636 = SURFACE_SIDE_STYLE ('',( #1371 ) ) ;
#2637 = EDGE_CURVE ( 'NONE', #850, #5253, #5278, .T. ) ;
#2638 = PRODUCT ( 'socket head cap screw_iso_ISO 4762 M12 x 80 - 36N', 'socket head cap screw_iso_ISO 4762 M12 x 80 - 36N', '', ( #1210 ) ) ;
#2639 = VERTEX_POINT ( 'NONE', #1883 ) ;
#2640 = DIRECTION ( 'NONE',  ( -0.000000000000000000, -0.000000000000000000, 1.000000000000000000 ) ) ;
#2641 = EDGE_CURVE ( 'NONE', #3240, #2438, #2944, .T. ) ;
#2642 = DIRECTION ( 'NONE',  ( 1.000000000000000000, -0.000000000000000000, 6.938893903907228378E-17 ) ) ;
#2643 = DIRECTION ( 'NONE',  ( -1.000000000000000000, -0.000000000000000000, -0.000000000000000000 ) ) ;
#2644 = AXIS2_PLACEMENT_3D ( 'NONE', #1986, #2037, #1250 ) ;
#2645 = EDGE_LOOP ( 'NONE', ( #3636, #1267, #993, #2090 ) ) ;
#2646 = ORIENTED_EDGE ( 'NONE', *, *, #2283, .F. ) ;
#2647 = CARTESIAN_POINT ( 'NONE',  ( 25.00000000000000000, 810.0000000000000000, -25.00000000000000000 ) ) ;
#2648 = FACE_OUTER_BOUND ( 'NONE', #1274, .T. ) ;
#2649 = CARTESIAN_POINT ( 'NONE',  ( -9.000000000000000000, -5.196152422706636465, -8.935996291721336249 ) ) ;
#2650 = CARTESIAN_POINT ( 'NONE',  ( -6.499999999999984901, 35.00000000000000000, 30.00000000000000711 ) ) ;
#2651 = AXIS2_PLACEMENT_3D ( 'NONE', #3669, #3249, #4493 ) ;
#2652 = CARTESIAN_POINT ( 'NONE',  ( 0.000000000000000000, 0.000000000000000000, 0.000000000000000000 ) ) ;
#2653 = ORIENTED_EDGE ( 'NONE', *, *, #5006, .F. ) ;
#2654 = CIRCLE ( 'NONE', #4387, 5.057500000000000107 ) ;
#2655 = CARTESIAN_POINT ( 'NONE',  ( 9.000000000000001776, 0.000000000000000000, 0.000000000000000000 ) ) ;
#2656 = DIRECTION ( 'NONE',  ( 1.000000000000000000, 0.000000000000000000, 0.000000000000000000 ) ) ;
#2657 = CARTESIAN_POINT ( 'NONE',  ( -150.0000000000000284, 0.000000000000000000, 149.9999999999999147 ) ) ;
#2658 = CARTESIAN_POINT ( 'NONE',  ( 0.000000000000000000, 330.0000000000000000, -25.00000000000000000 ) ) ;
#2659 = LINE ( 'NONE', #1386, #70 ) ;
#2660 = EDGE_LOOP ( 'NONE', ( #1262, #2891 ) ) ;
#2661 = AXIS2_PLACEMENT_3D ( 'NONE', #1552, #2854, #4938 ) ;
#2662 = EDGE_CURVE ( 'NONE', #4246, #3135, #5136, .T. ) ;
#2663 = VECTOR ( 'NONE', #675, 999.9999999999998863 ) ;
#2664 = CARTESIAN_POINT ( 'NONE',  ( -24.99999999999999645, 10.00000000000000000, -25.00000000000000000 ) ) ;
#2665 = CLOSED_SHELL ( 'NONE', ( #4635, #779, #4379, #1347, #3910, #5165 ) ) ;
#2666 = SURFACE_STYLE_FILL_AREA ( #3509 ) ;
#2667 = ORIENTED_EDGE ( 'NONE', *, *, #1736, .T. ) ;
#2668 = AXIS2_PLACEMENT_3D ( 'NONE', #585, #1073, #1911 ) ;
#2669 = STYLED_ITEM ( 'NONE', ( #1814 ), #3330 ) ;
#2670 = ORIENTED_EDGE ( 'NONE', *, *, #4181, .F. ) ;
#2671 = FACE_OUTER_BOUND ( 'NONE', #2400, .T. ) ;
#2672 = CONICAL_SURFACE ( 'NONE', #2757, 6.000000000000000000, 0.9599310885968784790 ) ;
#2673 = CARTESIAN_POINT ( 'NONE',  ( 11.99999999999999645, 0.000000000000000000, 0.000000000000000000 ) ) ;
#2674 = PRESENTATION_LAYER_ASSIGNMENT (  '', '', ( #5023 ) ) ;
#2675 = FACE_OUTER_BOUND ( 'NONE', #4210, .T. ) ;
#2676 = EDGE_LOOP ( 'NONE', ( #448, #1616, #2667, #5000 ) ) ;
#2677 = B_SPLINE_CURVE_WITH_KNOTS ( 'NONE', 3,
 ( #783, #1642, #2417, #3321, #4549, #1604 ),
 .UNSPECIFIED., .F., .F.,
 ( 4, 2, 4 ),
 ( 0.000000000000000000, 0.0005027859236379837553, 0.001005571847275967511 ),
 .UNSPECIFIED. ) ;
#2678 = ADVANCED_FACE ( 'NONE', ( #5219 ), #1909, .T. ) ;
#2679 = AXIS2_PLACEMENT_3D ( 'NONE', #4544, #3315, #823 ) ;
#2680 = ORIENTED_EDGE ( 'NONE', *, *, #266, .T. ) ;
#2681 = DIRECTION ( 'NONE',  ( 0.000000000000000000, 0.000000000000000000, -1.000000000000000000 ) ) ;
#2682 = DIRECTION ( 'NONE',  ( 1.850371707708594316E-16, 0.000000000000000000, -1.000000000000000000 ) ) ;
#2683 = DIRECTION ( 'NONE',  ( 1.000000000000000000, 0.000000000000000000, 0.000000000000000000 ) ) ;
#2684 = ORIENTED_EDGE ( 'NONE', *, *, #1878, .T. ) ;
#2685 = CARTESIAN_POINT ( 'NONE',  ( -25.00000000000000000, 60.00000000000000711, -25.00000000000000000 ) ) ;
#2686 = VECTOR ( 'NONE', #4009, 1000.000000000000000 ) ;
#2687 = CARTESIAN_POINT ( 'NONE',  ( -163.8084749684315966, 870.0000000000000000, 2.775557561562891351E-14 ) ) ;
#2688 = VECTOR ( 'NONE', #2900, 1000.000000000000000 ) ;
#2689 = FACE_BOUND ( 'NONE', #1124, .T. ) ;
#2690 = CARTESIAN_POINT ( 'NONE',  ( -150.0000000000000000, 885.0000000000000000, 25.00000000000000000 ) ) ;
#2691 = FACE_OUTER_BOUND ( 'NONE', #1045, .T. ) ;
#2692 = FACE_OUTER_BOUND ( 'NONE', #572, .T. ) ;
#2693 = DIRECTION ( 'NONE',  ( -1.000000000000000000, 0.000000000000000000, 0.000000000000000000 ) ) ;
#2694 = CIRCLE ( 'NONE', #1727, 6.499999999999988454 ) ;
#2695 = ADVANCED_FACE ( 'NONE', ( #4796 ), #2672, .F. ) ;
#2696 = B_SPLINE_CURVE_WITH_KNOTS ( 'NONE', 3,
 ( #5066, #3319, #967, #2224, #382, #5144 ),
 .UNSPECIFIED., .F., .F.,
 ( 4, 2, 4 ),
 ( 0.005538372264888902219, 0.008302394062588029644, 0.01106641586028715533 ),
 .UNSPECIFIED. ) ;
#2697 = DIRECTION ( 'NONE',  ( -0.000000000000000000, -0.000000000000000000, 1.000000000000000000 ) ) ;
#2698 = DIRECTION ( 'NONE',  ( -0.000000000000000000, -0.000000000000000000, 1.000000000000000000 ) ) ;
#2699 = SURFACE_SIDE_STYLE ('',( #2666 ) ) ;
#2700 = ORIENTED_EDGE ( 'NONE', *, *, #5071, .T. ) ;
#2701 = DIRECTION ( 'NONE',  ( -1.000000000000000000, -0.000000000000000000, -2.775557561562891351E-16 ) ) ;
#2702 = ORIENTED_EDGE ( 'NONE', *, *, #1496, .F. ) ;
#2703 = CARTESIAN_POINT ( 'NONE',  ( -6.499999999999988454, 450.0000000000000000, 25.00000000000000000 ) ) ;
#2704 = DIRECTION ( 'NONE',  ( -0.000000000000000000, -0.000000000000000000, 1.000000000000000000 ) ) ;
#2705 = EDGE_CURVE ( 'NONE', #2728, #2438, #1385, .T. ) ;
#2706 = ORIENTED_EDGE ( 'NONE', *, *, #4529, .F. ) ;
#2707 = LINE ( 'NONE', #5208, #3707 ) ;
#2708 = SURFACE_STYLE_FILL_AREA ( #3010 ) ;
#2709 = LINE ( 'NONE', #3082, #663 ) ;
#2710 = CARTESIAN_POINT ( 'NONE',  ( -25.00000000000000000, 10.00000000000000000, -25.00000000000000000 ) ) ;
#2711 = DIRECTION ( 'NONE',  ( 1.000000000000000000, 0.000000000000000000, 0.000000000000000000 ) ) ;
#2712 = EDGE_CURVE ( 'NONE', #4028, #1457, #3915, .T. ) ;
#2713 = DIRECTION ( 'NONE',  ( 1.000000000000000000, 0.000000000000000000, 0.000000000000000000 ) ) ;
#2714 = DIRECTION ( 'NONE',  ( -1.000000000000000000, 0.000000000000000000, 0.000000000000000000 ) ) ;
#2715 = LINE ( 'NONE', #628, #4928 ) ;
#2716 = CARTESIAN_POINT ( 'NONE',  ( -165.0000000000000000, 870.0000000000000000, 0.000000000000000000 ) ) ;
#2717 = DIRECTION ( 'NONE',  ( -0.000000000000000000, -0.000000000000000000, 1.000000000000000000 ) ) ;
#2718 = CARTESIAN_POINT ( 'NONE',  ( 9.000000000000000000, 4.737906595178606572, -8.848991057604585819 ) ) ;
#2719 = CARTESIAN_POINT ( 'NONE',  ( -2.352990130084610634E-16, 10.39230484541326582, -8.935996291721336249 ) ) ;
#2720 = ORIENTED_EDGE ( 'NONE', *, *, #4432, .F. ) ;
#2721 = EDGE_CURVE ( 'NONE', #3747, #5063, #3530, .T. ) ;
#2722 = EDGE_LOOP ( 'NONE', ( #2706, #3917, #3673 ) ) ;
#2723 = CARTESIAN_POINT ( 'NONE',  ( 6.000000000000000000, 5.839897972853065333, -6.938893903907228378E-15 ) ) ;
#2724 = ORIENTED_EDGE ( 'NONE', *, *, #1248, .T. ) ;
#2725 = CARTESIAN_POINT ( 'NONE',  ( 30.00000000000000355, 10.00000000000000000, 0.000000000000000000 ) ) ;
#2726 = CARTESIAN_POINT ( 'NONE',  ( 121.7157287525384533, -20.00000000000000000, 121.7157287525376859 ) ) ;
#2727 = EDGE_CURVE ( 'NONE', #3493, #338, #5159, .T. ) ;
#2728 = VERTEX_POINT ( 'NONE', #4767 ) ;
#2729 = EDGE_LOOP ( 'NONE', ( #3248, #1671, #2479, #4809 ) ) ;
#2730 = LINE ( 'NONE', #2316, #825 ) ;
#2731 = CARTESIAN_POINT ( 'NONE',  ( -25.00000000000000000, 610.0000000000000000, 24.99999999999999645 ) ) ;
#2732 = DIRECTION ( 'NONE',  ( 0.000000000000000000, 0.000000000000000000, -1.000000000000000000 ) ) ;
#2733 = DIRECTION ( 'NONE',  ( 1.000000000000000000, 0.000000000000000000, 0.000000000000000000 ) ) ;
#2734 = DIRECTION ( 'NONE',  ( 1.000000000000000000, 0.000000000000000000, 0.000000000000000000 ) ) ;
#2735 = CARTESIAN_POINT ( 'NONE',  ( 25.00000000000000000, 810.0000000000000000, -25.00000000000000000 ) ) ;
#2736 = AXIS2_PLACEMENT_3D ( 'NONE', #3726, #4078, #330 ) ;
#2737 = ORIENTED_EDGE ( 'NONE', *, *, #612, .T. ) ;
#2738 = SURFACE_STYLE_USAGE ( .BOTH. , #3560 ) ;
#2739 = CARTESIAN_POINT ( 'NONE',  ( -150.0000000000000000, 810.0000000000000000, -25.00000000000000000 ) ) ;
#2740 = DIRECTION ( 'NONE',  ( 1.000000000000000000, -0.000000000000000000, 2.081668171172168513E-16 ) ) ;
#2741 = CARTESIAN_POINT ( 'NONE',  ( 0.6000000000000033085, 0.000000000000000000, 0.000000000000000000 ) ) ;
#2742 = EDGE_CURVE ( 'NONE', #1196, #4486, #1048, .T. ) ;
#2743 = EDGE_CURVE ( 'NONE', #5225, #2280, #4393, .T. ) ;
#2744 = CARTESIAN_POINT ( 'NONE',  ( 8.999999999999998224, 4.659172099344154994, -9.367141211032262049 ) ) ;
#2745 = CARTESIAN_POINT ( 'NONE',  ( -139.9999999999999716, 820.0000000000001137, 25.00000000000000000 ) ) ;
#2746 = VECTOR ( 'NONE', #3144, 1000.000000000000000 ) ;
#2747 = ORIENTED_EDGE ( 'NONE', *, *, #1417, .F. ) ;
#2748 = AXIS2_PLACEMENT_3D ( 'NONE', #482, #2220, #2590 ) ;
#2749 = ORIENTED_EDGE ( 'NONE', *, *, #4120, .T. ) ;
#2750 = CLOSED_SHELL ( 'NONE', ( #1763, #2836, #802, #281, #964, #3594, #3, #5181, #2904, #2298, #2813, #5268, #1322, #4546, #2195, #4641, #1747, #4402, #4712, #2266, #1897, #1416, #58, #1706, #1699, #3318, #1557 ) ) ;
#2751 = FACE_BOUND ( 'NONE', #4970, .T. ) ;
#2752 = VERTEX_POINT ( 'NONE', #5249 ) ;
#2753 = DIRECTION ( 'NONE',  ( 1.000000000000000000, 0.000000000000000000, 0.000000000000000000 ) ) ;
#2754 = AXIS2_PLACEMENT_3D ( 'NONE', #5240, #3162, #4816 ) ;
#2755 = VECTOR ( 'NONE', #5251, 1000.000000000000000 ) ;
#2756 = CONICAL_SURFACE ( 'NONE', #3635, 5.010000000000002451, 0.9599310885968808105 ) ;
#2757 = AXIS2_PLACEMENT_3D ( 'NONE', #604, #4319, #3091 ) ;
#2758 = AXIS2_PLACEMENT_3D ( 'NONE', #4761, #1826, #1403 ) ;
#2759 = ORIENTED_EDGE ( 'NONE', *, *, #5286, .T. ) ;
#2760 = CARTESIAN_POINT ( 'NONE',  ( 6.499999999999981348, 35.00000000000000000, 25.00000000000000000 ) ) ;
#2761 = DIRECTION ( 'NONE',  ( -0.000000000000000000, 1.000000000000000000, -0.000000000000000000 ) ) ;
#2762 = AXIS2_PLACEMENT_3D ( 'NONE', #2574, #4232, #2154 ) ;
#2763 = CARTESIAN_POINT ( 'NONE',  ( 9.473745496805529243, 1.478328004173170497E-13, -9.138786188337405747 ) ) ;
#2764 = CARTESIAN_POINT ( 'NONE',  ( 0.000000000000000000, 570.0000000000000000, 30.00000000000000711 ) ) ;
#2765 = PRODUCT_CONTEXT ( 'NONE', #501, 'mechanical' ) ;
#2766 = VECTOR ( 'NONE', #4317, 1000.000000000000000 ) ;
#2767 = ORIENTED_EDGE ( 'NONE', *, *, #136, .T. ) ;
#2768 = CARTESIAN_POINT ( 'NONE',  ( -25.00000000000000000, 210.0000000000000284, 24.99999999999999645 ) ) ;
#2769 = CARTESIAN_POINT ( 'NONE',  ( -0.7810345657019083232, -10.51638858288774259, -9.518277236634766325 ) ) ;
#2770 = CARTESIAN_POINT ( 'NONE',  ( 3.049442433610978414E-16, 10.97743472985185775, -9.686084310752812954 ) ) ;
#2771 = AXIS2_PLACEMENT_3D ( 'NONE', #1740, #3974, #1471 ) ;
#2772 = DIRECTION ( 'NONE',  ( -1.000000000000000000, -0.000000000000000000, -0.000000000000000000 ) ) ;
#2773 = CARTESIAN_POINT ( 'NONE',  ( 6.000000000000000000, -2.919948986426526893, 5.057500000000001883 ) ) ;
#2774 = AXIS2_PLACEMENT_3D ( 'NONE', #528, #2586, #1317 ) ;
#2775 = ADVANCED_FACE ( 'NONE', ( #3170 ), #4003, .F. ) ;
#2776 = EDGE_CURVE ( 'NONE', #1575, #3569, #550, .T. ) ;
#2777 = CARTESIAN_POINT ( 'NONE',  ( -150.0000000000000000, 870.0000000000000000, 0.000000000000000000 ) ) ;
#2778 = DIRECTION ( 'NONE',  ( -0.000000000000000000, -1.000000000000000000, 0.000000000000000000 ) ) ;
#2779 = VECTOR ( 'NONE', #1487, 1000.000000000000000 ) ;
#2780 = ORIENTED_EDGE ( 'NONE', *, *, #1705, .F. ) ;
#2781 = PLANE ( 'NONE',  #5014 ) ;
#2782 = CARTESIAN_POINT ( 'NONE',  ( -17.99999999999999645, -3.469446951953614189E-15, -12.00000000000000000 ) ) ;
#2783 = ORIENTED_EDGE ( 'NONE', *, *, #2305, .T. ) ;
#2784 = DIRECTION ( 'NONE',  ( -0.000000000000000000, 1.000000000000000000, -0.000000000000000000 ) ) ;
#2785 = DIRECTION ( 'NONE',  ( 1.000000000000000000, 0.000000000000000000, 0.000000000000000000 ) ) ;
#2786 = ORIENTED_EDGE ( 'NONE', *, *, #2341, .T. ) ;
#2787 = FACE_OUTER_BOUND ( 'NONE', #1820, .T. ) ;
#2788 = CARTESIAN_POINT ( 'NONE',  ( -3.954162315725865184, -8.656288888418751881, -9.137374534099176770 ) ) ;
#2789 = FACE_BOUND ( 'NONE', #4125, .T. ) ;
#2790 = DIRECTION ( 'NONE',  ( 0.000000000000000000, 0.000000000000000000, 1.000000000000000000 ) ) ;
#2791 = PRODUCT_CONTEXT ( 'NONE', #287, 'mechanical' ) ;
#2792 = EDGE_CURVE ( 'NONE', #1641, #2863, #3019, .T. ) ;
#2793 = ORIENTED_EDGE ( 'NONE', *, *, #1218, .T. ) ;
#2794 = EDGE_CURVE ( 'NONE', #3050, #4571, #2313, .T. ) ;
#2795 = DIRECTION ( 'NONE',  ( -1.000000000000000000, -0.000000000000000000, -0.000000000000000000 ) ) ;
#2796 = FACE_OUTER_BOUND ( 'NONE', #294, .T. ) ;
#2797 = CARTESIAN_POINT ( 'NONE',  ( -150.0000000000000284, 10.00000000000000000, -150.0000000000000853 ) ) ;
#2798 = DIRECTION ( 'NONE',  ( 0.000000000000000000, 0.000000000000000000, 1.000000000000000000 ) ) ;
#2799 = DIRECTION ( 'NONE',  ( 0.000000000000000000, 1.000000000000000000, -1.188187522481193495E-15 ) ) ;
#2800 = DIRECTION ( 'NONE',  ( 1.000000000000000000, 0.000000000000000000, 0.000000000000000000 ) ) ;
#2801 = CARTESIAN_POINT ( 'NONE',  ( 9.000000000000003553, 3.464101615137751722, -8.667800885990208926 ) ) ;
#2802 = ORIENTED_EDGE ( 'NONE', *, *, #2473, .F. ) ;
#2803 = ORIENTED_EDGE ( 'NONE', *, *, #632, .F. ) ;
#2804 = AXIS2_PLACEMENT_3D ( 'NONE', #4734, #1772, #1016 ) ;
#2805 =( REPRESENTATION_RELATIONSHIP ('NONE','NONE', #4791, #1634 ) REPRESENTATION_RELATIONSHIP_WITH_TRANSFORMATION ( #1235 )SHAPE_REPRESENTATION_RELATIONSHIP( ) );
#2806 = ORIENTED_EDGE ( 'NONE', *, *, #708, .T. ) ;
#2807 = DIRECTION ( 'NONE',  ( 0.000000000000000000, 0.000000000000000000, -1.000000000000000000 ) ) ;
#2808 = ORIENTED_EDGE ( 'NONE', *, *, #2721, .T. ) ;
#2809 = PRODUCT_DEFINITION_SHAPE ( 'NONE', 'NONE',  #5390 ) ;
#2810 = ORIENTED_EDGE ( 'NONE', *, *, #1670, .T. ) ;
#2811 = EDGE_CURVE ( 'NONE', #273, #3402, #3638, .T. ) ;
#2812 = B_SPLINE_CURVE_WITH_KNOTS ( 'NONE', 3,
 ( #4795, #3484, #549, #3886, #3965, #2191, #222, #3861 ),
 .UNSPECIFIED., .F., .F.,
 ( 4, 2, 2, 4 ),
 ( 2.475501736912785259E-07, 0.002666746755945495657, 0.003999996358831399076, 0.005333245961717302495 ),
 .UNSPECIFIED. ) ;
#2813 = ADVANCED_FACE ( 'NONE', ( #1644 ), #4926, .T. ) ;
#2814 = VERTEX_POINT ( 'NONE', #4884 ) ;
#2815 = CARTESIAN_POINT ( 'NONE',  ( 121.7157287525372311, 0.000000000000000000, -136.7157287525388085 ) ) ;
#2816 = CARTESIAN_POINT ( 'NONE',  ( 150.0000000000000000, 885.0000000000000000, 25.00000000000000000 ) ) ;
#2817 = DIRECTION ( 'NONE',  ( 1.000000000000000000, 0.000000000000000000, 0.000000000000000000 ) ) ;
#2818 = CARTESIAN_POINT ( 'NONE',  ( 0.000000000000000000, 510.0000000000000000, -25.00000000000000000 ) ) ;
#2819 = APPLICATION_PROTOCOL_DEFINITION ( 'draft international standard', 'automotive_design', 1998, #4768 ) ;
#2820 = DIRECTION ( 'NONE',  ( 0.000000000000000000, -0.000000000000000000, 1.000000000000000000 ) ) ;
#2821 = DIRECTION ( 'NONE',  ( -0.000000000000000000, -0.000000000000000000, 1.000000000000000000 ) ) ;
#2822 = FACE_OUTER_BOUND ( 'NONE', #4974, .T. ) ;
#2823 = DIRECTION ( 'NONE',  ( 1.000000000000000000, 0.000000000000000000, 0.000000000000000000 ) ) ;
#2824 = PRODUCT_DEFINITION_CONTEXT ( 'detailed design', #5061, 'design' ) ;
#2825 = CARTESIAN_POINT ( 'NONE',  ( -8.249999999999998224, -5.629165124598855208, -8.787392856021023491 ) ) ;
#2826 = VECTOR ( 'NONE', #1303, 1000.000000000000000 ) ;
#2827 = ORIENTED_EDGE ( 'NONE', *, *, #1041, .F. ) ;
#2828 = DIRECTION ( 'NONE',  ( 1.000000000000000000, 0.000000000000000000, 0.000000000000000000 ) ) ;
#2829 = UNCERTAINTY_MEASURE_WITH_UNIT (LENGTH_MEASURE( 1.000000000000000082E-05 ), #2615, 'distance_accuracy_value', 'NONE');
#2830 = LINE ( 'NONE', #4452, #771 ) ;
#2831 = ORIENTED_EDGE ( 'NONE', *, *, #3391, .T. ) ;
#2832 =( NAMED_UNIT ( * ) SI_UNIT ( $, .STERADIAN. ) SOLID_ANGLE_UNIT ( ) );
#2833 = ORIENTED_EDGE ( 'NONE', *, *, #11, .T. ) ;
#2834 = CIRCLE ( 'NONE', #1503, 6.499999999999993783 ) ;
#2835 = EDGE_LOOP ( 'NONE', ( #4044, #702, #2990, #1164, #1079 ) ) ;
#2836 = ADVANCED_FACE ( 'NONE', ( #3293 ), #3378, .T. ) ;
#2837 = EDGE_LOOP ( 'NONE', ( #347, #3969, #3702, #3549 ) ) ;
#2838 = VECTOR ( 'NONE', #2640, 1000.000000000000000 ) ;
#2839 = EDGE_LOOP ( 'NONE', ( #1401, #41, #5005, #3370, #4197 ) ) ;
#2840 = FACE_OUTER_BOUND ( 'NONE', #2202, .T. ) ;
#2841 = EDGE_LOOP ( 'NONE', ( #4565, #4978 ) ) ;
#2842 = DIRECTION ( 'NONE',  ( -0.000000000000000000, -0.000000000000000000, 1.000000000000000000 ) ) ;
#2843 = CIRCLE ( 'NONE', #997, 15.00000000000000000 ) ;
#2844 = EDGE_LOOP ( 'NONE', ( #2803, #2504, #3241 ) ) ;
#2845 = AXIS2_PLACEMENT_3D ( 'NONE', #988, #2697, #3567 ) ;
#2846 = CARTESIAN_POINT ( 'NONE',  ( -150.0000000000000000, 870.0000000000000000, 5.999999999999950262 ) ) ;
#2847 = EDGE_CURVE ( 'NONE', #261, #5260, #2057, .T. ) ;
#2848 = CARTESIAN_POINT ( 'NONE',  ( -3.145560420647206978, -9.127459525683745412, -9.189462574975419074 ) ) ;
#2849 = MECHANICAL_DESIGN_GEOMETRIC_PRESENTATION_REPRESENTATION (  '', ( #4730 ), #1782 ) ;
#2850 = DIRECTION ( 'NONE',  ( 0.000000000000000000, 0.000000000000000000, -1.000000000000000000 ) ) ;
#2851 = CARTESIAN_POINT ( 'NONE',  ( 12.38940648156203750, 0.000000000000000000, -10.20000000000000107 ) ) ;
#2852 = SHAPE_DEFINITION_REPRESENTATION ( #4294, #4791 ) ;
#2853 =( GEOMETRIC_REPRESENTATION_CONTEXT ( 3 ) GLOBAL_UNCERTAINTY_ASSIGNED_CONTEXT ( ( #3044 ) ) GLOBAL_UNIT_ASSIGNED_CONTEXT ( ( #5031, #2555, #1312 ) ) REPRESENTATION_CONTEXT ( 'NONE', 'WORKASPACE' ) );
#2854 = DIRECTION ( 'NONE',  ( -0.000000000000000000, -0.000000000000000000, 1.000000000000000000 ) ) ;
#2855 = ORIENTED_EDGE ( 'NONE', *, *, #470, .F. ) ;
#2856 = CARTESIAN_POINT ( 'NONE',  ( 0.000000000000000000, 0.000000000000000000, -12.00000000000000000 ) ) ;
#2857 = DIRECTION ( 'NONE',  ( -0.000000000000000000, -0.000000000000000000, -1.000000000000000000 ) ) ;
#2858 = DIRECTION ( 'NONE',  ( 1.000000000000000000, 0.000000000000000000, 2.081668171172168513E-16 ) ) ;
#2859 = CARTESIAN_POINT ( 'NONE',  ( 8.716590831518757909, 5.934788533967490842, -9.518202542148554102 ) ) ;
#2860 = AXIS2_PLACEMENT_3D ( 'NONE', #1925, #739, #2407 ) ;
#2861 = AXIS2_PLACEMENT_3D ( 'NONE', #1486, #3643, #1207 ) ;
#2862 = PRESENTATION_LAYER_ASSIGNMENT (  '', '', ( #67 ) ) ;
#2863 = VERTEX_POINT ( 'NONE', #1933 ) ;
#2864 = FACE_OUTER_BOUND ( 'NONE', #1650, .T. ) ;
#2865 = DIRECTION ( 'NONE',  ( 0.000000000000000000, 0.000000000000000000, 1.000000000000000000 ) ) ;
#2866 = B_SPLINE_CURVE_WITH_KNOTS ( 'NONE', 3,
 ( #4510, #790, #2451, #4116, #368, #2026, #3712, #1613, #3302 ),
 .UNSPECIFIED., .F., .F.,
 ( 4, 2, 1, 2, 4 ),
 ( 0.000000000000000000, 0.002598076211353316737, 0.005196152422706633474, 0.007794228634059948910, 0.01039230484541326521 ),
 .UNSPECIFIED. ) ;
#2867 = ORIENTED_EDGE ( 'NONE', *, *, #5214, .F. ) ;
#2868 = VERTEX_POINT ( 'NONE', #3678 ) ;
#2869 = EDGE_LOOP ( 'NONE', ( #3781, #3510, #1532, #735 ) ) ;
#2870 = AXIS2_PLACEMENT_3D ( 'NONE', #3824, #2698, #2250 ) ;
#2871 = ORIENTED_EDGE ( 'NONE', *, *, #5198, .F. ) ;
#2872 = EDGE_CURVE ( 'NONE', #5260, #2556, #5275, .T. ) ;
#2873 = B_SPLINE_CURVE_WITH_KNOTS ( 'NONE', 3,
 ( #1327, #4650, #923, #2181, #3852, #105 ),
 .UNSPECIFIED., .F., .F.,
 ( 4, 2, 4 ),
 ( 0.005538372264888893545, 0.008302394062588022705, 0.01106641586028715360 ),
 .UNSPECIFIED. ) ;
#2874 = ADVANCED_FACE ( 'NONE', ( #363, #2447, #4059 ), #4134, .F. ) ;
#2875 = AXIS2_PLACEMENT_3D ( 'NONE', #1645, #831, #3758 ) ;
#2876 = EDGE_CURVE ( 'NONE', #4428, #4982, #226, .T. ) ;
#2877 = DIRECTION ( 'NONE',  ( 0.000000000000000000, 0.000000000000000000, -1.000000000000000000 ) ) ;
#2878 = ORIENTED_EDGE ( 'NONE', *, *, #1136, .F. ) ;
#2879 =( NAMED_UNIT ( * ) PLANE_ANGLE_UNIT ( ) SI_UNIT ( $, .RADIAN. ) );
#2880 = AXIS2_PLACEMENT_3D ( 'NONE', #204, #5171, #1788 ) ;
#2881 = ORIENTED_EDGE ( 'NONE', *, *, #4163, .T. ) ;
#2882 = DIRECTION ( 'NONE',  ( -1.000000000000000000, 0.000000000000000000, -0.000000000000000000 ) ) ;
#2883 = LINE ( 'NONE', #4573, #5112 ) ;
#2884 = FACE_BOUND ( 'NONE', #4150, .T. ) ;
#2885 = LINE ( 'NONE', #1208, #2156 ) ;
#2886 = UNCERTAINTY_MEASURE_WITH_UNIT (LENGTH_MEASURE( 1.000000000000000082E-05 ), #2204, 'distance_accuracy_value', 'NONE');
#2887 = PRODUCT_CONTEXT ( 'NONE', #109, 'mechanical' ) ;
#2888 = EDGE_CURVE ( 'NONE', #3489, #1575, #1964, .T. ) ;
#2889 = ORIENTED_EDGE ( 'NONE', *, *, #1762, .T. ) ;
#2890 = LINE ( 'NONE', #3650, #5172 ) ;
#2891 = ORIENTED_EDGE ( 'NONE', *, *, #4540, .F. ) ;
#2892 = DIRECTION ( 'NONE',  ( 0.000000000000000000, 0.000000000000000000, 1.000000000000000000 ) ) ;
#2893 = DIRECTION ( 'NONE',  ( 0.000000000000000000, 0.000000000000000000, 1.000000000000000000 ) ) ;
#2894 = CARTESIAN_POINT ( 'NONE',  ( 0.000000000000000000, 450.0000000000000000, -25.00000000000000000 ) ) ;
#2895 = LINE ( 'NONE', #4528, #1629 ) ;
#2896 = EDGE_CURVE ( 'NONE', #3300, #5294, #4834, .T. ) ;
#2897 = ADVANCED_FACE ( 'NONE', ( #1555, #5308 ), #388, .F. ) ;
#2898 = VERTEX_POINT ( 'NONE', #4968 ) ;
#2899 = CYLINDRICAL_SURFACE ( 'NONE', #484, 6.499999999999988454 ) ;
#2900 = DIRECTION ( 'NONE',  ( 1.000000000000000000, 0.000000000000000000, 2.081668171172168513E-16 ) ) ;
#2901 = ORIENTED_EDGE ( 'NONE', *, *, #3232, .F. ) ;
#2902 = ORIENTED_EDGE ( 'NONE', *, *, #3480, .F. ) ;
#2903 = DIRECTION ( 'NONE',  ( 0.000000000000000000, 0.000000000000000000, 1.000000000000000000 ) ) ;
#2904 = ADVANCED_FACE ( 'NONE', ( #2418, #4088 ), #4942, .T. ) ;
#2905 = EDGE_LOOP ( 'NONE', ( #3955, #2310, #3666, #3907, #3452, #444, #4149 ) ) ;
#2906 = ORIENTED_EDGE ( 'NONE', *, *, #3921, .F. ) ;
#2907 = CIRCLE ( 'NONE', #4273, 20.00000000000001421 ) ;
#2908 = ORIENTED_EDGE ( 'NONE', *, *, #691, .F. ) ;
#2909 = CARTESIAN_POINT ( 'NONE',  ( 6.000000000000000000, -2.919948986426539772, -5.057499999999996554 ) ) ;
#2910 = CARTESIAN_POINT ( 'NONE',  ( -139.9999999999999716, 820.0000000000001137, 25.00000000000000000 ) ) ;
#2911 = DIRECTION ( 'NONE',  ( 0.000000000000000000, 1.000000000000000000, 0.000000000000000000 ) ) ;
#2912 = CYLINDRICAL_SURFACE ( 'NONE', #1723, 6.000000000000000888 ) ;
#2913 = EDGE_CURVE ( 'NONE', #754, #3765, #2137, .T. ) ;
#2914 = DIRECTION ( 'NONE',  ( 0.000000000000000000, -1.000000000000000000, 0.000000000000000000 ) ) ;
#2915 = ORIENTED_EDGE ( 'NONE', *, *, #3208, .T. ) ;
#2916 = PLANE ( 'NONE',  #679 ) ;
#2917 = DIRECTION ( 'NONE',  ( 1.000000000000000000, -0.000000000000000000, 6.938893903907228378E-17 ) ) ;
#2918 = DIRECTION ( 'NONE',  ( 1.000000000000000000, 0.000000000000000000, 0.000000000000000000 ) ) ;
#2919 = CARTESIAN_POINT ( 'NONE',  ( -9.000000000000000000, -3.727046135536770777, -9.220349054170952741 ) ) ;
#2920 = ORIENTED_EDGE ( 'NONE', *, *, #3190, .F. ) ;
#2921 = APPLICATION_CONTEXT ( 'automotive_design' ) ;
#2922 = ORIENTED_EDGE ( 'NONE', *, *, #3767, .T. ) ;
#2923 = DIRECTION ( 'NONE',  ( -5.551115123125753120E-16, -1.000000000000000000, 0.000000000000000000 ) ) ;
#2924 = DIRECTION ( 'NONE',  ( 0.000000000000000000, 0.000000000000000000, 1.000000000000000000 ) ) ;
#2925 = EDGE_LOOP ( 'NONE', ( #4124, #1450, #4407, #3749 ) ) ;
#2926 = ADVANCED_FACE ( 'NONE', ( #1606 ), #2503, .T. ) ;
#2927 = EDGE_LOOP ( 'NONE', ( #5310, #4777, #2810, #4852 ) ) ;
#2928 = EDGE_CURVE ( 'NONE', #5042, #1919, #3191, .T. ) ;
#2929 = CYLINDRICAL_SURFACE ( 'NONE', #4396, 6.499999999999988454 ) ;
#2930 = AXIS2_PLACEMENT_3D ( 'NONE', #1681, #968, #4255 ) ;
#2931 = ORIENTED_EDGE ( 'NONE', *, *, #3062, .F. ) ;
#2932 = AXIS2_PLACEMENT_3D ( 'NONE', #3419, #4183, #1356 ) ;
#2933 = ORIENTED_EDGE ( 'NONE', *, *, #3232, .T. ) ;
#2934 = SHAPE_REPRESENTATION ( 'socket head cap screw_iso_ISO 4762 M12 x 80 - 36N', ( #4154 ), #2853 ) ;
#2935 = CYLINDRICAL_SURFACE ( 'NONE', #1502, 20.00000000000001421 ) ;
#2936 = LINE ( 'NONE', #30, #584 ) ;
#2937 = DIRECTION ( 'NONE',  ( -0.000000000000000000, -0.000000000000000000, 1.000000000000000000 ) ) ;
#2938 = CONICAL_SURFACE ( 'NONE', #122, 5.057500000000000107, 1.047197551196592302 ) ;
#2939 = AXIS2_PLACEMENT_3D ( 'NONE', #3273, #5009, #4563 ) ;
#2940 = DIRECTION ( 'NONE',  ( 1.000000000000000000, 0.000000000000000000, 0.000000000000000000 ) ) ;
#2941 = AXIS2_PLACEMENT_3D ( 'NONE', #703, #1537, #2530 ) ;
#2942 = CARTESIAN_POINT ( 'NONE',  ( -6.000000000000000000, 0.000000000000000000, -11.97459999999999880 ) ) ;
#2943 = CARTESIAN_POINT ( 'NONE',  ( -9.000000000000000000, 5.581228263432454817, -9.543753411584054547 ) ) ;
#2944 = CIRCLE ( 'NONE', #5016, 6.499999999999988454 ) ;
#2945 =( GEOMETRIC_REPRESENTATION_CONTEXT ( 3 ) GLOBAL_UNCERTAINTY_ASSIGNED_CONTEXT ( ( #2506 ) ) GLOBAL_UNIT_ASSIGNED_CONTEXT ( ( #431, #2251, #4710 ) ) REPRESENTATION_CONTEXT ( 'NONE', 'WORKASPACE' ) );
#2946 = ADVANCED_BREP_SHAPE_REPRESENTATION ( '', ( #3645, #4154 ), #3368 ) ;
#2947 = AXIS2_PLACEMENT_3D ( 'NONE', #90, #2157, #1746 ) ;
#2948 = ORIENTED_EDGE ( 'NONE', *, *, #1387, .T. ) ;
#2949 = EDGE_LOOP ( 'NONE', ( #2827, #2474, #1712, #2452 ) ) ;
#2950 = CARTESIAN_POINT ( 'NONE',  ( 0.000000000000000000, 0.000000000000000000, 0.000000000000000000 ) ) ;
#2951 = UNCERTAINTY_MEASURE_WITH_UNIT (LENGTH_MEASURE( 1.000000000000000082E-05 ), #669, 'distance_accuracy_value', 'NONE');
#2952 = CARTESIAN_POINT ( 'NONE',  ( 0.000000000000000000, 510.0000000000000000, 25.00000000000000000 ) ) ;
#2953 = ORIENTED_EDGE ( 'NONE', *, *, #4271, .T. ) ;
#2954 = VERTEX_POINT ( 'NONE', #2498 ) ;
#2955 = EDGE_CURVE ( 'NONE', #963, #4457, #1710, .T. ) ;
#2956 = CARTESIAN_POINT ( 'NONE',  ( 4.894105558640191589, -7.566691683689909631, -3.942938369468767290E-15 ) ) ;
#2957 = VERTEX_POINT ( 'NONE', #881 ) ;
#2958 = VECTOR ( 'NONE', #1987, 1000.000000000000000 ) ;
#2959 = VECTOR ( 'NONE', #986, 1000.000000000000000 ) ;
#2960 = ORIENTED_EDGE ( 'NONE', *, *, #2007, .F. ) ;
#2961 = DIRECTION ( 'NONE',  ( 0.000000000000000000, 0.000000000000000000, 1.000000000000000000 ) ) ;
#2962 = LINE ( 'NONE', #3394, #928 ) ;
#2963 = CARTESIAN_POINT ( 'NONE',  ( 5.519484922003871752, -7.752549460314996921, -9.137374534099006240 ) ) ;
#2964 = CARTESIAN_POINT ( 'NONE',  ( 5.035999999999988042, 570.0000000000000000, -24.99999999999998579 ) ) ;
#2965 = DIRECTION ( 'NONE',  ( -1.000000000000000000, 0.000000000000000000, 0.000000000000000000 ) ) ;
#2966 = CARTESIAN_POINT ( 'NONE',  ( -4.105894441359819069, -8.021765584429989104, -4.008159906407348416E-15 ) ) ;
#2967 = DIRECTION ( 'NONE',  ( 0.000000000000000000, -1.000000000000000000, 0.000000000000000000 ) ) ;
#2968 = EDGE_CURVE ( 'NONE', #3516, #4353, #2099, .T. ) ;
#2969 = EDGE_CURVE ( 'NONE', #1160, #1575, #4626, .T. ) ;
#2970 = ORIENTED_EDGE ( 'NONE', *, *, #4395, .T. ) ;
#2971 = DIRECTION ( 'NONE',  ( 1.000000000000000000, -0.000000000000000000, 0.000000000000000000 ) ) ;
#2972 = PLANE ( 'NONE',  #4090 ) ;
#2973 = EDGE_LOOP ( 'NONE', ( #579, #1625, #2304, #161 ) ) ;
#2974 = EDGE_CURVE ( 'NONE', #2814, #3262, #274, .T. ) ;
#2975 = DIRECTION ( 'NONE',  ( 0.000000000000000000, 0.000000000000000000, -1.000000000000000000 ) ) ;
#2976 = ORIENTED_EDGE ( 'NONE', *, *, #2712, .F. ) ;
#2977 = EDGE_LOOP ( 'NONE', ( #3928, #267, #1298, #1611 ) ) ;
#2978 = VERTEX_POINT ( 'NONE', #898 ) ;
#2979 = FACE_OUTER_BOUND ( 'NONE', #5232, .T. ) ;
#2980 = CARTESIAN_POINT ( 'NONE',  ( -25.00000000000000000, 60.00000000000000711, -25.00000000000000000 ) ) ;
#2981 = CARTESIAN_POINT ( 'NONE',  ( 6.331831610933278398, -7.287864996261299133, -9.189462574975568288 ) ) ;
#2982 = EDGE_CURVE ( 'NONE', #3493, #3135, #36, .T. ) ;
#2983 = EDGE_CURVE ( 'NONE', #2404, #285, #2421, .T. ) ;
#2984 = CARTESIAN_POINT ( 'NONE',  ( -9.000000000000000000, 1.787897550172801830, -0.1425508600568100859 ) ) ;
#2985 = ORIENTED_EDGE ( 'NONE', *, *, #4857, .T. ) ;
#2986 = CARTESIAN_POINT ( 'NONE',  ( -74.99999999999998579, 610.0000000000000000, 49.99999999999998579 ) ) ;
#2987 = DIRECTION ( 'NONE',  ( 0.000000000000000000, 0.000000000000000000, 1.000000000000000000 ) ) ;
#2988 = AXIS2_PLACEMENT_3D ( 'NONE', #2994, #1805, #3913 ) ;
#2989 = DIRECTION ( 'NONE',  ( 1.000000000000000000, 0.000000000000000000, 2.081668171172168513E-16 ) ) ;
#2990 = ORIENTED_EDGE ( 'NONE', *, *, #1481, .T. ) ;
#2991 = CARTESIAN_POINT ( 'NONE',  ( -9.489862997586008930, -3.701980733639088417, -9.383919243293616930 ) ) ;
#2992 = PRESENTATION_STYLE_ASSIGNMENT (( #469 ) ) ;
#2993 = EDGE_LOOP ( 'NONE', ( #479, #5282, #2802, #4598 ) ) ;
#2994 = CARTESIAN_POINT ( 'NONE',  ( 139.9999999999999716, 870.0000000000000000, 0.000000000000000000 ) ) ;
#2995 = DIRECTION ( 'NONE',  ( -1.000000000000000000, -0.000000000000000000, -0.000000000000000000 ) ) ;
#2996 = UNCERTAINTY_MEASURE_WITH_UNIT (LENGTH_MEASURE( 1.000000000000000082E-05 ), #5130, 'distance_accuracy_value', 'NONE');
#2997 = CARTESIAN_POINT ( 'NONE',  ( -121.7157287525381122, 0.000000000000000000, 136.7157287525380127 ) ) ;
#2998 = LINE ( 'NONE', #4194, #3450 ) ;
#2999 = PRODUCT_RELATED_PRODUCT_CATEGORY ( 'part', '', ( #1749 ) ) ;
#3000 = AXIS2_PLACEMENT_3D ( 'NONE', #971, #5099, #1821 ) ;
#3001 = CIRCLE ( 'NONE', #1333, 0.5999999999999998668 ) ;
#3002 = ORIENTED_EDGE ( 'NONE', *, *, #4409, .F. ) ;
#3003 = DIRECTION ( 'NONE',  ( -1.000000000000000000, -0.000000000000000000, -0.000000000000000000 ) ) ;
#3004 = DIRECTION ( 'NONE',  ( -0.000000000000000000, -1.000000000000000000, -0.000000000000000000 ) ) ;
#3005 = CARTESIAN_POINT ( 'NONE',  ( 7.784221022415031221, -5.898082742690404778, -8.707326526324870031 ) ) ;
#3006 = AXIS2_PLACEMENT_3D ( 'NONE', #2594, #536, #1713 ) ;
#3007 = EDGE_CURVE ( 'NONE', #1075, #4782, #3890, .T. ) ;
#3008 = LINE ( 'NONE', #3369, #1771 ) ;
#3009 = CARTESIAN_POINT ( 'NONE',  ( 6.000000000000000000, -4.379923479639794337, 2.528750000000003606 ) ) ;
#3010 = FILL_AREA_STYLE ('',( #3519 ) ) ;
#3011 = FACE_OUTER_BOUND ( 'NONE', #2905, .T. ) ;
#3012 = ORIENTED_EDGE ( 'NONE', *, *, #2955, .F. ) ;
#3013 = FACE_BOUND ( 'NONE', #20, .T. ) ;
#3014 = AXIS2_PLACEMENT_3D ( 'NONE', #402, #4980, #4099 ) ;
#3015 = VERTEX_POINT ( 'NONE', #3401 ) ;
#3016 = DIRECTION ( 'NONE',  ( 0.000000000000000000, 0.000000000000000000, -1.000000000000000000 ) ) ;
#3017 = DIRECTION ( 'NONE',  ( 0.000000000000000000, 0.000000000000000000, -1.000000000000000000 ) ) ;
#3018 = ORIENTED_EDGE ( 'NONE', *, *, #4529, .T. ) ;
#3019 = CIRCLE ( 'NONE', #1276, 6.499999999999988454 ) ;
#3020 = AXIS2_PLACEMENT_3D ( 'NONE', #4701, #1462, #3524 ) ;
#3021 = CARTESIAN_POINT ( 'NONE',  ( 0.000000000000000000, 5.839897972853065333, -6.938893903907228378E-15 ) ) ;
#3022 = EDGE_CURVE ( 'NONE', #2639, #4261, #59, .T. ) ;
#3023 =( NAMED_UNIT ( * ) SI_UNIT ( $, .STERADIAN. ) SOLID_ANGLE_UNIT ( ) );
#3024 = AXIS2_PLACEMENT_3D ( 'NONE', #4107, #356, #4933 ) ;
#3025 = EDGE_CURVE ( 'NONE', #1856, #1919, #5049, .T. ) ;
#3026 = AXIS2_PLACEMENT_3D ( 'NONE', #3904, #2682, #3496 ) ;
#3027 = ORIENTED_EDGE ( 'NONE', *, *, #3277, .T. ) ;
#3028 = CARTESIAN_POINT ( 'NONE',  ( -9.000000000000000000, -5.196152422706636465, -1.199999999999999734 ) ) ;
#3029 = CARTESIAN_POINT ( 'NONE',  ( -31.74999999999995737, 0.000000000000000000, 0.000000000000000000 ) ) ;
#3030 = CARTESIAN_POINT ( 'NONE',  ( 92.00000000000000000, 5.035999999999999588, 0.000000000000000000 ) ) ;
#3031 = AXIS2_PLACEMENT_3D ( 'NONE', #2217, #5220, #4394 ) ;
#3032 = CARTESIAN_POINT ( 'NONE',  ( 12.59999999999999964, 0.000000000000000000, 0.000000000000000000 ) ) ;
#3033 = ORIENTED_EDGE ( 'NONE', *, *, #1827, .T. ) ;
#3034 = CARTESIAN_POINT ( 'NONE',  ( -1.676835913137321903E-15, 35.00000000000000000, 25.00000000000000000 ) ) ;
#3035 = LINE ( 'NONE', #1822, #3108 ) ;
#3036 = CARTESIAN_POINT ( 'NONE',  ( -150.0000000000000284, 10.00000000000000000, -150.0000000000000853 ) ) ;
#3037 = DIRECTION ( 'NONE',  ( -0.000000000000000000, -0.000000000000000000, 1.000000000000000000 ) ) ;
#3038 = EDGE_CURVE ( 'NONE', #2539, #4929, #1349, .T. ) ;
#3039 = CARTESIAN_POINT ( 'NONE',  ( -121.7157287525392917, -20.00000000000000000, -136.7157287525368190 ) ) ;
#3040 = VERTEX_POINT ( 'NONE', #498 ) ;
#3041 = CARTESIAN_POINT ( 'NONE',  ( 121.7157287525384533, 0.000000000000000000, 121.7157287525376859 ) ) ;
#3042 = CARTESIAN_POINT ( 'NONE',  ( 6.499999999999988454, 390.0000000000000000, -25.00000000000000000 ) ) ;
#3043 = FACE_OUTER_BOUND ( 'NONE', #26, .T. ) ;
#3044 = UNCERTAINTY_MEASURE_WITH_UNIT (LENGTH_MEASURE( 1.000000000000000082E-05 ), #5031, 'distance_accuracy_value', 'NONE');
#3045 = DIRECTION ( 'NONE',  ( 1.000000000000000000, 0.000000000000000000, 0.000000000000000000 ) ) ;
#3046 = ADVANCED_FACE ( 'NONE', ( #4551, #4264 ), #5028, .F. ) ;
#3047 = VERTEX_POINT ( 'NONE', #1767 ) ;
#3048 = EDGE_CURVE ( 'NONE', #4454, #4028, #522, .T. ) ;
#3049 = CARTESIAN_POINT ( 'NONE',  ( 6.052010058236154677, -6.898175209152300091, -0.1432599722966034494 ) ) ;
#3050 = VERTEX_POINT ( 'NONE', #2553 ) ;
#3051 = LINE ( 'NONE', #4254, #989 ) ;
#3052 = LINE ( 'NONE', #125, #2826 ) ;
#3053 = FACE_OUTER_BOUND ( 'NONE', #3585, .T. ) ;
#3054 = CIRCLE ( 'NONE', #1916, 15.00000000000000000 ) ;
#3055 = FACE_OUTER_BOUND ( 'NONE', #1728, .T. ) ;
#3056 = ORIENTED_EDGE ( 'NONE', *, *, #156, .F. ) ;
#3057 = ORIENTED_EDGE ( 'NONE', *, *, #2613, .F. ) ;
#3058 = CARTESIAN_POINT ( 'NONE',  ( -25.00000000000000000, 60.00000000000000711, -25.00000000000000000 ) ) ;
#3059 = CARTESIAN_POINT ( 'NONE',  ( -150.0000000000000284, 0.000000000000000000, -150.0000000000000853 ) ) ;
#3060 = CARTESIAN_POINT ( 'NONE',  ( -9.000000000000005329, -1.732050807568881634, -8.505011083697297636 ) ) ;
#3061 = CARTESIAN_POINT ( 'NONE',  ( 0.000000000000000000, 390.0000000000000000, 25.00000000000000000 ) ) ;
#3062 = EDGE_CURVE ( 'NONE', #5291, #745, #2225, .T. ) ;
#3063 = VECTOR ( 'NONE', #2203, 1000.000000000000000 ) ;
#3064 = AXIS2_PLACEMENT_3D ( 'NONE', #5157, #1752, #1729 ) ;
#3065 = FACE_OUTER_BOUND ( 'NONE', #2844, .T. ) ;
#3066 =( LENGTH_UNIT ( ) NAMED_UNIT ( * ) SI_UNIT ( .MILLI., .METRE. ) );
#3067 = DIRECTION ( 'NONE',  ( 0.000000000000000000, 1.000000000000000000, 0.000000000000000000 ) ) ;
#3068 = DIRECTION ( 'NONE',  ( -0.000000000000000000, -0.000000000000000000, 1.000000000000000000 ) ) ;
#3069 = DIRECTION ( 'NONE',  ( 1.000000000000000000, 0.000000000000000000, 0.000000000000000000 ) ) ;
#3070 = CARTESIAN_POINT ( 'NONE',  ( 9.507374323136149386, 5.554569297917910653, -9.698322317877195786 ) ) ;
#3071 = EDGE_CURVE ( 'NONE', #2556, #1702, #830, .T. ) ;
#3072 = ORIENTED_EDGE ( 'NONE', *, *, #5072, .F. ) ;
#3073 = LINE ( 'NONE', #4691, #2838 ) ;
#3074 =( REPRESENTATION_RELATIONSHIP ('NONE','NONE', #4791, #1634 ) REPRESENTATION_RELATIONSHIP_WITH_TRANSFORMATION ( #3848 )SHAPE_REPRESENTATION_RELATIONSHIP( ) );
#3075 = CARTESIAN_POINT ( 'NONE',  ( 6.499999999999988454, 330.0000000000000000, 25.00000000000000000 ) ) ;
#3076 = CARTESIAN_POINT ( 'NONE',  ( -9.000000000000000000, -5.196152422706636465, -8.935996291721336249 ) ) ;
#3077 = CIRCLE ( 'NONE', #1588, 6.000000000000001776 ) ;
#3078 = VERTEX_POINT ( 'NONE', #4205 ) ;
#3079 = VERTEX_POINT ( 'NONE', #465 ) ;
#3080 = DIRECTION ( 'NONE',  ( 0.000000000000000000, 0.000000000000000000, -1.000000000000000000 ) ) ;
#3081 = DIRECTION ( 'NONE',  ( 0.000000000000000000, -0.000000000000000000, 1.000000000000000000 ) ) ;
#3082 = CARTESIAN_POINT ( 'NONE',  ( 0.000000000000000000, -10.39230484541327293, -12.00000000000000000 ) ) ;
#3083 = EDGE_LOOP ( 'NONE', ( #2346, #449, #2027, #941, #3987, #3719 ) ) ;
#3084 = CARTESIAN_POINT ( 'NONE',  ( -31.74999999999995737, 1.102182119232617714E-15, -9.000000000000000000 ) ) ;
#3085 = VECTOR ( 'NONE', #262, 1000.000000000000000 ) ;
#3086 = CARTESIAN_POINT ( 'NONE',  ( 0.000000000000000000, 0.000000000000000000, 0.000000000000000000 ) ) ;
#3087 = VECTOR ( 'NONE', #4733, 1000.000000000000000 ) ;
#3088 = LINE ( 'NONE', #953, #4562 ) ;
#3089 = DIRECTION ( 'NONE',  ( -0.000000000000000000, 1.000000000000000000, -0.000000000000000000 ) ) ;
#3090 = CARTESIAN_POINT ( 'NONE',  ( -139.9999999999999716, 810.0000000000000000, -25.00000000000000000 ) ) ;
#3091 = DIRECTION ( 'NONE',  ( -1.000000000000000000, 0.000000000000000000, 0.000000000000000000 ) ) ;
#3092 = LINE ( 'NONE', #4004, #150 ) ;
#3093 = CIRCLE ( 'NONE', #1601, 6.499999999999988454 ) ;
#3094 = CARTESIAN_POINT ( 'NONE',  ( 9.000000000000000000, -3.788589235757911844, -9.200462692535689158 ) ) ;
#3095 = DIRECTION ( 'NONE',  ( -0.000000000000000000, -1.000000000000000000, -0.000000000000000000 ) ) ;
#3096 = CLOSED_SHELL ( 'NONE', ( #5140, #2327, #2775, #4770, #3514, #4826, #305, #3388, #3411, #4018, #5385, #3597, #875, #5096, #4619, #2056 ) ) ;
#3097 = VECTOR ( 'NONE', #3804, 1000.000000000000000 ) ;
#3098 = ADVANCED_FACE ( 'NONE', ( #3011 ), #1188, .T. ) ;
#3099 = ORIENTED_EDGE ( 'NONE', *, *, #5007, .F. ) ;
#3100 = EDGE_LOOP ( 'NONE', ( #3537, #2780 ) ) ;
#3101 = CARTESIAN_POINT ( 'NONE',  ( -1.676835913137321903E-15, 35.00000000000000000, 30.00000000000000711 ) ) ;
#3102 = VECTOR ( 'NONE', #696, 1000.000000000000000 ) ;
#3103 = ORIENTED_EDGE ( 'NONE', *, *, #2624, .T. ) ;
#3104 = LINE ( 'NONE', #4839, #3358 ) ;
#3105 = AXIS2_PLACEMENT_3D ( 'NONE', #603, #1848, #3528 ) ;
#3106 = DIRECTION ( 'NONE',  ( 1.000000000000000000, 0.000000000000000000, 0.000000000000000000 ) ) ;
#3107 = CIRCLE ( 'NONE', #1198, 20.00000000000001421 ) ;
#3108 = VECTOR ( 'NONE', #4263, 1000.000000000000000 ) ;
#3109 = APPLICATION_CONTEXT ( 'automotive_design' ) ;
#3110 = ORIENTED_EDGE ( 'NONE', *, *, #1212, .T. ) ;
#3111 = ORIENTED_EDGE ( 'NONE', *, *, #4698, .T. ) ;
#3112 = CARTESIAN_POINT ( 'NONE',  ( -8.281895533831891143, 5.610750229555061530, -0.8426663529491297266 ) ) ;
#3113 = PLANE ( 'NONE',  #670 ) ;
#3114 = FACE_OUTER_BOUND ( 'NONE', #2977, .T. ) ;
#3115 = LINE ( 'NONE', #2650, #680 ) ;
#3116 = VECTOR ( 'NONE', #3124, 1000.000000000000114 ) ;
#3117 = DIRECTION ( 'NONE',  ( 0.000000000000000000, 0.000000000000000000, 1.000000000000000000 ) ) ;
#3118 = VECTOR ( 'NONE', #3363, 1000.000000000000000 ) ;
#3119 = ADVANCED_FACE ( 'NONE', ( #3114 ), #2625, .F. ) ;
#3120 = DIRECTION ( 'NONE',  ( 5.551115123125753120E-16, 1.000000000000000000, 1.155557966632335381E-31 ) ) ;
#3121 = CARTESIAN_POINT ( 'NONE',  ( -8.716590831518756133, -5.934788533967497948, -9.518202542148552325 ) ) ;
#3122 = DIRECTION ( 'NONE',  ( 0.000000000000000000, 0.000000000000000000, 1.000000000000000000 ) ) ;
#3123 = DIRECTION ( 'NONE',  ( 0.000000000000000000, -0.5000000000000008882, -0.8660254037844380415 ) ) ;
#3124 = DIRECTION ( 'NONE',  ( 0.000000000000000000, -0.4999999999999991118, 0.8660254037844390407 ) ) ;
#3125 = AXIS2_PLACEMENT_3D ( 'NONE', #4087, #2892, #2940 ) ;
#3126 = EDGE_CURVE ( 'NONE', #3765, #5063, #1435, .T. ) ;
#3127 = CARTESIAN_POINT ( 'NONE',  ( 9.507358203129939511, -5.552904979773809480, -9.698011706630772721 ) ) ;
#3128 = CARTESIAN_POINT ( 'NONE',  ( 0.000000000000000000, 570.0000000000000000, 30.00000000000000711 ) ) ;
#3129 = EDGE_CURVE ( 'NONE', #4595, #338, #3521, .T. ) ;
#3130 = ORIENTED_EDGE ( 'NONE', *, *, #3874, .T. ) ;
#3131 = CARTESIAN_POINT ( 'NONE',  ( 12.00000000000000000, 0.000000000000000000, -6.600000000000001421 ) ) ;
#3132 = ORIENTED_EDGE ( 'NONE', *, *, #1106, .F. ) ;
#3133 = DIRECTION ( 'NONE',  ( 0.000000000000000000, 0.000000000000000000, 1.000000000000000000 ) ) ;
#3134 = LINE ( 'NONE', #2228, #2337 ) ;
#3135 = VERTEX_POINT ( 'NONE', #1871 ) ;
#3136 = DIRECTION ( 'NONE',  ( -0.8660254037844383745, 0.5000000000000003331, 0.000000000000000000 ) ) ;
#3137 = CARTESIAN_POINT ( 'NONE',  ( -9.416515850482078065, -4.955676884309061947, -9.021433408186455338 ) ) ;
#3138 = DIRECTION ( 'NONE',  ( -1.000000000000000000, 0.000000000000000000, 0.000000000000000000 ) ) ;
#3139 = ADVANCED_FACE ( 'NONE', ( #3581 ), #4787, .F. ) ;
#3140 = DIRECTION ( 'NONE',  ( -1.000000000000000000, -0.000000000000000000, -0.000000000000000000 ) ) ;
#3141 = DIRECTION ( 'NONE',  ( 0.000000000000000000, 0.000000000000000000, 1.000000000000000000 ) ) ;
#3142 = EDGE_CURVE ( 'NONE', #1457, #3821, #2318, .T. ) ;
#3143 = ORIENTED_EDGE ( 'NONE', *, *, #80, .F. ) ;
#3144 = DIRECTION ( 'NONE',  ( -0.000000000000000000, 1.000000000000000000, -0.000000000000000000 ) ) ;
#3145 = LINE ( 'NONE', #3588, #4531 ) ;
#3146 = DIRECTION ( 'NONE',  ( 0.8191520442889902442, 1.003171929053522651E-16, -0.5735764363510483799 ) ) ;
#3147 = CARTESIAN_POINT ( 'NONE',  ( -121.7157287525392917, -20.00000000000000000, -121.7157287525368332 ) ) ;
#3148 = CARTESIAN_POINT ( 'NONE',  ( 6.499999999999981348, 35.00000000000000000, 30.00000000000000711 ) ) ;
#3149 = ORIENTED_EDGE ( 'NONE', *, *, #3022, .T. ) ;
#3150 = FACE_OUTER_BOUND ( 'NONE', #3165, .T. ) ;
#3151 = CARTESIAN_POINT ( 'NONE',  ( -9.000000000000001776, 0.000000000000000000, 0.000000000000000000 ) ) ;
#3152 = ORIENTED_EDGE ( 'NONE', *, *, #2562, .F. ) ;
#3153 = DIRECTION ( 'NONE',  ( 0.000000000000000000, 0.000000000000000000, -1.000000000000000000 ) ) ;
#3154 = VERTEX_POINT ( 'NONE', #1359 ) ;
#3155 = LINE ( 'NONE', #2725, #3269 ) ;
#3156 = ORIENTED_EDGE ( 'NONE', *, *, #665, .T. ) ;
#3157 = ORIENTED_EDGE ( 'NONE', *, *, #1081, .F. ) ;
#3158 = CYLINDRICAL_SURFACE ( 'NONE', #2113, 5.999999999999996447 ) ;
#3159 = FACE_OUTER_BOUND ( 'NONE', #2676, .T. ) ;
#3160 = FACE_OUTER_BOUND ( 'NONE', #4913, .T. ) ;
#3161 = DIRECTION ( 'NONE',  ( -0.000000000000000000, 1.000000000000000000, -0.000000000000000000 ) ) ;
#3162 = DIRECTION ( 'NONE',  ( 1.224646799147353207E-16, -4.064521778635712183E-50, -1.000000000000000000 ) ) ;
#3163 = ADVANCED_FACE ( 'NONE', ( #3991 ), #597, .T. ) ;
#3164 = ORIENTED_EDGE ( 'NONE', *, *, #737, .F. ) ;
#3165 = EDGE_LOOP ( 'NONE', ( #3278, #1001, #3220, #902, #1473 ) ) ;
#3166 = DIRECTION ( 'NONE',  ( 0.8660254037844383745, -0.5000000000000003331, 0.000000000000000000 ) ) ;
#3167 = AXIS2_PLACEMENT_3D ( 'NONE', #5125, #1744, #5074 ) ;
#3168 = DIRECTION ( 'NONE',  ( 0.000000000000000000, 0.000000000000000000, -1.000000000000000000 ) ) ;
#3169 = DIRECTION ( 'NONE',  ( -1.000000000000000000, 0.000000000000000000, 0.000000000000000000 ) ) ;
#3170 = FACE_OUTER_BOUND ( 'NONE', #286, .T. ) ;
#3171 = CARTESIAN_POINT ( 'NONE',  ( -4.500000000000000000, -7.794228634059951588, -8.419403919045803875 ) ) ;
#3172 = AXIS2_PLACEMENT_3D ( 'NONE', #515, #4224, #5067 ) ;
#3173 = CYLINDRICAL_SURFACE ( 'NONE', #5095, 5.999999999999950262 ) ;
#3174 = LINE ( 'NONE', #4831, #1534 ) ;
#3175 = VECTOR ( 'NONE', #5304, 1000.000000000000000 ) ;
#3176 = ORIENTED_EDGE ( 'NONE', *, *, #2968, .F. ) ;
#3177 = ORIENTED_EDGE ( 'NONE', *, *, #310, .T. ) ;
#3178 = B_SPLINE_CURVE_WITH_KNOTS ( 'NONE', 3,
 ( #2288, #4021, #5261, #5149, #3956, #1869 ),
 .UNSPECIFIED., .F., .F.,
 ( 4, 2, 4 ),
 ( -5.636559625666465778E-06, 0.0004989239064927809787, 0.001003484372611228564 ),
 .UNSPECIFIED. ) ;
#3179 = VECTOR ( 'NONE', #5113, 1000.000000000000000 ) ;
#3180 = EDGE_LOOP ( 'NONE', ( #1429, #3341, #4444, #1837 ) ) ;
#3181 = CIRCLE ( 'NONE', #839, 5.035999999999999588 ) ;
#3182 = LINE ( 'NONE', #4778, #5012 ) ;
#3183 = ADVANCED_FACE ( 'NONE', ( #1062, #2262, #3958 ), #1040, .T. ) ;
#3184 = ORIENTED_EDGE ( 'NONE', *, *, #2974, .F. ) ;
#3185 = DIRECTION ( 'NONE',  ( 2.081668171172168513E-16, 0.000000000000000000, -1.000000000000000000 ) ) ;
#3186 = PRODUCT_DEFINITION_FORMATION_WITH_SPECIFIED_SOURCE ( 'ANY', '', #976, .NOT_KNOWN. ) ;
#3187 = CARTESIAN_POINT ( 'NONE',  ( 6.000000000000000000, 5.839897972853065333, -6.938893903907228378E-15 ) ) ;
#3188 = AXIS2_PLACEMENT_3D ( 'NONE', #3887, #629, #3562 ) ;
#3189 =( GEOMETRIC_REPRESENTATION_CONTEXT ( 3 ) GLOBAL_UNCERTAINTY_ASSIGNED_CONTEXT ( ( #1990 ) ) GLOBAL_UNIT_ASSIGNED_CONTEXT ( ( #1626, #1203, #3276 ) ) REPRESENTATION_CONTEXT ( 'NONE', 'WORKASPACE' ) );
#3190 = EDGE_CURVE ( 'NONE', #4714, #183, #5190, .T. ) ;
#3191 = CIRCLE ( 'NONE', #575, 6.000000000000000000 ) ;
#3192 = ORIENTED_EDGE ( 'NONE', *, *, #3025, .T. ) ;
#3193 = CARTESIAN_POINT ( 'NONE',  ( 149.9999999999999716, 10.00000000000000000, 149.9999999999999716 ) ) ;
#3194 = CARTESIAN_POINT ( 'NONE',  ( -2.865539685210635845, -8.737884736783355422, -8.512883888440837765 ) ) ;
#3195 = CARTESIAN_POINT ( 'NONE',  ( 139.9999999999999716, 870.0000000000000000, 5.999999999999950262 ) ) ;
#3196 = CARTESIAN_POINT ( 'NONE',  ( 92.00000000000000000, 0.000000000000000000, 0.000000000000000000 ) ) ;
#3197 = AXIS2_PLACEMENT_3D ( 'NONE', #1795, #4307, #1286 ) ;
#3198 = UNCERTAINTY_MEASURE_WITH_UNIT (LENGTH_MEASURE( 1.000000000000000082E-05 ), #3688, 'distance_accuracy_value', 'NONE');
#3199 = APPLICATION_PROTOCOL_DEFINITION ( 'draft international standard', 'automotive_design', 1998, #3404 ) ;
#3200 = VECTOR ( 'NONE', #5218, 1000.000000000000000 ) ;
#3201 = LINE ( 'NONE', #2354, #557 ) ;
#3202 = FACE_BOUND ( 'NONE', #1703, .T. ) ;
#3203 = DIRECTION ( 'NONE',  ( -1.000000000000000000, 0.000000000000000000, -0.000000000000000000 ) ) ;
#3204 = AXIS2_PLACEMENT_3D ( 'NONE', #1328, #1664, #1721 ) ;
#3205 = CARTESIAN_POINT ( 'NONE',  ( -24.99999999999999645, 210.0000000000000284, -25.00000000000000000 ) ) ;
#3206 = LINE ( 'NONE', #1130, #3307 ) ;
#3207 = VECTOR ( 'NONE', #1243, 1000.000000000000000 ) ;
#3208 = EDGE_CURVE ( 'NONE', #4028, #1510, #5127, .T. ) ;
#3209 = B_SPLINE_CURVE_WITH_KNOTS ( 'NONE', 3,
 ( #2441, #3696, #1120, #713, #270, #2763 ),
 .UNSPECIFIED., .F., .F.,
 ( 4, 2, 4 ),
 ( 0.000000000000000000, 0.002769186132444446773, 0.005538372264888893545 ),
 .UNSPECIFIED. ) ;
#3210 = DIRECTION ( 'NONE',  ( -0.000000000000000000, -0.000000000000000000, 1.000000000000000000 ) ) ;
#3211 = DIRECTION ( 'NONE',  ( 1.000000000000000000, 0.000000000000000000, 0.000000000000000000 ) ) ;
#3212 = CIRCLE ( 'NONE', #5303, 5.057500000000000107 ) ;
#3213 = ORIENTED_EDGE ( 'NONE', *, *, #5105, .F. ) ;
#3214 = EDGE_CURVE ( 'NONE', #5213, #5234, #416, .T. ) ;
#3215 = ORIENTED_EDGE ( 'NONE', *, *, #2983, .T. ) ;
#3216 = EDGE_CURVE ( 'NONE', #2509, #3920, #1843, .T. ) ;
#3217 = ORIENTED_EDGE ( 'NONE', *, *, #4327, .T. ) ;
#3218 = VERTEX_POINT ( 'NONE', #4360 ) ;
#3219 = CARTESIAN_POINT ( 'NONE',  ( -9.473745496805529243, -1.478735707944909295E-13, -9.138786188337405747 ) ) ;
#3220 = ORIENTED_EDGE ( 'NONE', *, *, #4656, .F. ) ;
#3221 = CARTESIAN_POINT ( 'NONE',  ( 0.000000000000000000, 610.0000000000000000, 0.000000000000000000 ) ) ;
#3222 = SURFACE_SIDE_STYLE ('',( #3692 ) ) ;
#3223 = EDGE_LOOP ( 'NONE', ( #2004, #3413, #4678, #3541 ) ) ;
#3224 = DIRECTION ( 'NONE',  ( -1.387778780781445676E-16, 0.000000000000000000, -1.000000000000000000 ) ) ;
#3225 = DIRECTION ( 'NONE',  ( -0.000000000000000000, 1.000000000000000000, -0.000000000000000000 ) ) ;
#3226 = DIRECTION ( 'NONE',  ( 0.000000000000000000, 0.000000000000000000, 1.000000000000000000 ) ) ;
#3227 = CARTESIAN_POINT ( 'NONE',  ( 6.000000000000000000, 0.000000000000000000, 0.000000000000000000 ) ) ;
#3228 = PRODUCT_CONTEXT ( 'NONE', #2167, 'mechanical' ) ;
#3229 = ORIENTED_EDGE ( 'NONE', *, *, #3447, .F. ) ;
#3230 = FACE_OUTER_BOUND ( 'NONE', #2722, .T. ) ;
#3231 = CARTESIAN_POINT ( 'NONE',  ( -3.945874696944569937, 8.661172281173762144, -9.138600484129256074 ) ) ;
#3232 = EDGE_CURVE ( 'NONE', #4982, #791, #571, .T. ) ;
#3233 = DIRECTION ( 'NONE',  ( -1.000000000000000000, -0.000000000000000000, -0.000000000000000000 ) ) ;
#3234 = CARTESIAN_POINT ( 'NONE',  ( -5.999999999999999112, -6.928203230275515878, -8.505011083697295859 ) ) ;
#3235 = ORIENTED_EDGE ( 'NONE', *, *, #2211, .T. ) ;
#3236 = FACE_OUTER_BOUND ( 'NONE', #3714, .T. ) ;
#3237 = CARTESIAN_POINT ( 'NONE',  ( -150.0000000000000284, 10.00000000000000000, 149.9999999999999147 ) ) ;
#3238 = EDGE_LOOP ( 'NONE', ( #770, #2535, #4482, #1535 ) ) ;
#3239 = EDGE_LOOP ( 'NONE', ( #1245, #135, #4629, #2285, #4881 ) ) ;
#3240 = VERTEX_POINT ( 'NONE', #1400 ) ;
#3241 = ORIENTED_EDGE ( 'NONE', *, *, #1528, .F. ) ;
#3242 = EDGE_CURVE ( 'NONE', #3078, #1225, #2709, .T. ) ;
#3243 = DIRECTION ( 'NONE',  ( -1.000000000000000000, -7.401486830834378251E-16, -2.081668171172168513E-16 ) ) ;
#3244 = LINE ( 'NONE', #3332, #2044 ) ;
#3245 = EDGE_CURVE ( 'NONE', #3573, #4209, #3543, .T. ) ;
#3246 = VERTEX_POINT ( 'NONE', #5349 ) ;
#3247 = ORIENTED_EDGE ( 'NONE', *, *, #4597, .F. ) ;
#3248 = ORIENTED_EDGE ( 'NONE', *, *, #1980, .T. ) ;
#3249 = DIRECTION ( 'NONE',  ( -1.000000000000000000, -0.000000000000000000, -0.000000000000000000 ) ) ;
#3250 = CARTESIAN_POINT ( 'NONE',  ( 8.283033339518244276, 5.610093317135758539, -0.8432325327665438630 ) ) ;
#3251 = CARTESIAN_POINT ( 'NONE',  ( 150.0000000000000000, 870.0000000000000000, 0.000000000000000000 ) ) ;
#3252 = DIRECTION ( 'NONE',  ( 0.000000000000000000, 0.000000000000000000, -1.000000000000000000 ) ) ;
#3253 = UNCERTAINTY_MEASURE_WITH_UNIT (LENGTH_MEASURE( 1.000000000000000082E-05 ), #4, 'distance_accuracy_value', 'NONE');
#3254 = PRODUCT_CONTEXT ( 'NONE', #5160, 'mechanical' ) ;
#3255 = CARTESIAN_POINT ( 'NONE',  ( 0.000000000000000000, 610.0000000000000000, -30.00000000000000355 ) ) ;
#3256 = ORIENTED_EDGE ( 'NONE', *, *, #563, .F. ) ;
#3257 = LINE ( 'NONE', #4940, #1628 ) ;
#3258 = CARTESIAN_POINT ( 'NONE',  ( 165.0000000000000000, 870.0000000000000000, 0.000000000000000000 ) ) ;
#3259 = DIRECTION ( 'NONE',  ( -0.000000000000000000, -0.000000000000000000, 1.000000000000000000 ) ) ;
#3260 = EDGE_CURVE ( 'NONE', #813, #2382, #4658, .T. ) ;
#3261 = CARTESIAN_POINT ( 'NONE',  ( 5.527857873577811887, 7.747813868291101080, -9.138600484129261403 ) ) ;
#3262 = VERTEX_POINT ( 'NONE', #2349 ) ;
#3263 = AXIS2_PLACEMENT_3D ( 'NONE', #1739, #29, #3846 ) ;
#3264 = EDGE_LOOP ( 'NONE', ( #2345, #4775 ) ) ;
#3265 = DIRECTION ( 'NONE',  ( 0.000000000000000000, 0.000000000000000000, 1.000000000000000000 ) ) ;
#3266 = CARTESIAN_POINT ( 'NONE',  ( 9.000000000000000000, 5.196152422706629359, -8.935996291721334472 ) ) ;
#3267 = VERTEX_POINT ( 'NONE', #3284 ) ;
#3268 = EDGE_LOOP ( 'NONE', ( #2831, #1294, #5124, #2062 ) ) ;
#3269 = VECTOR ( 'NONE', #203, 1000.000000000000000 ) ;
#3270 = VERTEX_POINT ( 'NONE', #298 ) ;
#3271 = ORIENTED_EDGE ( 'NONE', *, *, #3038, .T. ) ;
#3272 = CIRCLE ( 'NONE', #2121, 5.057500000000000107 ) ;
#3273 = CARTESIAN_POINT ( 'NONE',  ( 0.000000000000000000, 0.000000000000000000, -12.00000000000000000 ) ) ;
#3274 = VERTEX_POINT ( 'NONE', #1952 ) ;
#3275 = SHAPE_REPRESENTATION ( 'Vertical Telescoping Support Column', ( #4154 ), #5370 ) ;
#3276 =( NAMED_UNIT ( * ) SI_UNIT ( $, .STERADIAN. ) SOLID_ANGLE_UNIT ( ) );
#3277 = EDGE_CURVE ( 'NONE', #2529, #4400, #1197, .T. ) ;
#3278 = ORIENTED_EDGE ( 'NONE', *, *, #110, .T. ) ;
#3279 = PRODUCT_DEFINITION_FORMATION_WITH_SPECIFIED_SOURCE ( 'ANY', '', #1749, .NOT_KNOWN. ) ;
#3280 = VERTEX_POINT ( 'NONE', #5325 ) ;
#3281 = VECTOR ( 'NONE', #1019, 1000.000000000000000 ) ;
#3282 = DIRECTION ( 'NONE',  ( -1.000000000000000000, -0.000000000000000000, -0.000000000000000000 ) ) ;
#3283 = CARTESIAN_POINT ( 'NONE',  ( -8.603171985749405337, 5.425261183556192357, -8.848996304170942295 ) ) ;
#3284 = CARTESIAN_POINT ( 'NONE',  ( -25.00000000000000000, 60.00000000000000711, 25.00000000000000000 ) ) ;
#3285 = DIRECTION ( 'NONE',  ( 1.000000000000000000, 0.000000000000000000, 0.000000000000000000 ) ) ;
#3286 = EDGE_CURVE ( 'NONE', #4279, #2752, #2321, .T. ) ;
#3287 = VECTOR ( 'NONE', #3373, 1000.000000000000114 ) ;
#3288 =( GEOMETRIC_REPRESENTATION_CONTEXT ( 3 ) GLOBAL_UNCERTAINTY_ASSIGNED_CONTEXT ( ( #3812 ) ) GLOBAL_UNIT_ASSIGNED_CONTEXT ( ( #3759, #3375, #500 ) ) REPRESENTATION_CONTEXT ( 'NONE', 'WORKASPACE' ) );
#3289 = CARTESIAN_POINT ( 'NONE',  ( -31.74999999999995737, 0.000000000000000000, 6.000000000000001776 ) ) ;
#3290 = ORIENTED_EDGE ( 'NONE', *, *, #1044, .F. ) ;
#3291 = FACE_OUTER_BOUND ( 'NONE', #4091, .T. ) ;
#3292 = FILL_AREA_STYLE_COLOUR ( '', #2143 ) ;
#3293 = FACE_OUTER_BOUND ( 'NONE', #4603, .T. ) ;
#3294 = CARTESIAN_POINT ( 'NONE',  ( 6.000000000000000000, -5.839897972853064445, 4.770489558936219510E-15 ) ) ;
#3295 = AXIS2_PLACEMENT_3D ( 'NONE', #3932, #4677, #213 ) ;
#3296 = CIRCLE ( 'NONE', #2322, 6.499999999999993783 ) ;
#3297 = ORIENTED_EDGE ( 'NONE', *, *, #4012, .T. ) ;
#3298 = EDGE_CURVE ( 'NONE', #3154, #3303, #2142, .T. ) ;
#3299 = CIRCLE ( 'NONE', #3816, 6.000000000000000000 ) ;
#3300 = VERTEX_POINT ( 'NONE', #1569 ) ;
#3301 = DIRECTION ( 'NONE',  ( 1.000000000000000000, 0.000000000000000000, 0.000000000000000000 ) ) ;
#3302 = CARTESIAN_POINT ( 'NONE',  ( -9.000000000000000000, 5.196152422706629359, -8.935996291721334472 ) ) ;
#3303 = VERTEX_POINT ( 'NONE', #4080 ) ;
#3304 = ORIENTED_EDGE ( 'NONE', *, *, #2091, .F. ) ;
#3305 = AXIS2_PLACEMENT_3D ( 'NONE', #4349, #2271, #1998 ) ;
#3306 = EDGE_LOOP ( 'NONE', ( #343, #2083, #608, #594 ) ) ;
#3307 = VECTOR ( 'NONE', #2799, 1000.000000000000000 ) ;
#3308 = CARTESIAN_POINT ( 'NONE',  ( 0.000000000000000000, 390.0000000000000000, 25.00000000000000000 ) ) ;
#3309 = ORIENTED_EDGE ( 'NONE', *, *, #1496, .T. ) ;
#3310 = EDGE_CURVE ( 'NONE', #4535, #4898, #3107, .T. ) ;
#3311 = VECTOR ( 'NONE', #1840, 1000.000000000000000 ) ;
#3312 = ORIENTED_EDGE ( 'NONE', *, *, #2928, .F. ) ;
#3313 = LINE ( 'NONE', #5323, #2032 ) ;
#3314 = LINE ( 'NONE', #436, #4937 ) ;
#3315 = DIRECTION ( 'NONE',  ( 2.081668171172168513E-16, 0.000000000000000000, -1.000000000000000000 ) ) ;
#3316 = CARTESIAN_POINT ( 'NONE',  ( 12.59999999999999964, 7.347880794884121708E-16, -6.000000000000001776 ) ) ;
#3317 = PRODUCT_CONTEXT ( 'NONE', #2458, 'mechanical' ) ;
#3318 = ADVANCED_FACE ( 'NONE', ( #3160 ), #2375, .F. ) ;
#3319 = CARTESIAN_POINT ( 'NONE',  ( -9.473745496805527466, 0.9176529770164936206, -9.138786188337402194 ) ) ;
#3320 = ORIENTED_EDGE ( 'NONE', *, *, #1212, .F. ) ;
#3321 = CARTESIAN_POINT ( 'NONE',  ( -1.020776138296702871E-15, -10.67487845244187206, -9.530716183751497539 ) ) ;
#3322 = DIRECTION ( 'NONE',  ( -1.000000000000000000, 0.000000000000000000, -2.081668171172168513E-16 ) ) ;
#3323 = ADVANCED_FACE ( 'NONE', ( #4521, #3608, #1514, #2884, #1089 ), #4495, .T. ) ;
#3324 = CARTESIAN_POINT ( 'NONE',  ( -150.0000000000000284, 10.00000000000000000, 149.9999999999999147 ) ) ;
#3325 = ORIENTED_EDGE ( 'NONE', *, *, #4103, .F. ) ;
#3326 = CARTESIAN_POINT ( 'NONE',  ( 149.9999999999999716, 0.000000000000000000, 149.9999999999999716 ) ) ;
#3327 = CARTESIAN_POINT ( 'NONE',  ( 121.7157287525372311, -20.00000000000000000, -106.7157287525388369 ) ) ;
#3328 = ORIENTED_EDGE ( 'NONE', *, *, #4657, .T. ) ;
#3329 = ORIENTED_EDGE ( 'NONE', *, *, #2662, .T. ) ;
#3330 = ADVANCED_BREP_SHAPE_REPRESENTATION ( '', ( #47, #4154 ), #2055 ) ;
#3331 = ORIENTED_EDGE ( 'NONE', *, *, #4800, .F. ) ;
#3332 = CARTESIAN_POINT ( 'NONE',  ( -121.7157287525392917, -20.00000000000000000, -106.7157287525368332 ) ) ;
#3333 = ORIENTED_EDGE ( 'NONE', *, *, #2414, .F. ) ;
#3334 = FILL_AREA_STYLE_COLOUR ( '', #2501 ) ;
#3335 = ORIENTED_EDGE ( 'NONE', *, *, #3667, .T. ) ;
#3336 = ORIENTED_EDGE ( 'NONE', *, *, #2969, .F. ) ;
#3337 = LINE ( 'NONE', #4899, #4215 ) ;
#3338 = CARTESIAN_POINT ( 'NONE',  ( -8.534985340083300898, 5.464628761784600997, -9.367146555589094703 ) ) ;
#3339 = CARTESIAN_POINT ( 'NONE',  ( 9.564083412974087040, -5.456344092479600505, -9.698321917585792207 ) ) ;
#3340 = ITEM_DEFINED_TRANSFORMATION ( 'NONE', 'NONE', #4568,  #4154 ) ;
#3341 = ORIENTED_EDGE ( 'NONE', *, *, #787, .T. ) ;
#3342 = CARTESIAN_POINT ( 'NONE',  ( -150.0000000000000000, 820.0000000000001137, 25.00000000000000000 ) ) ;
#3343 = DIRECTION ( 'NONE',  ( 1.000000000000000000, 0.000000000000000000, 0.000000000000000000 ) ) ;
#3344 = CARTESIAN_POINT ( 'NONE',  ( 9.000000000000000000, -5.196152422706636465, -8.935996291721336249 ) ) ;
#3345 = SHAPE_REPRESENTATION_RELATIONSHIP ( 'NONE' , 'NONE' ,  #1634, #1615 ) ;
#3346 = ADVANCED_FACE ( 'NONE', ( #1546 ), #4440, .F. ) ;
#3347 = EDGE_LOOP ( 'NONE', ( #1302, #759, #5368, #1824 ) ) ;
#3348 = EDGE_LOOP ( 'NONE', ( #455, #397, #4195, #1757 ) ) ;
#3349 = CARTESIAN_POINT ( 'NONE',  ( 6.403089491456118054, 7.242747656091411024, -9.141698485140111075 ) ) ;
#3350 = CYLINDRICAL_SURFACE ( 'NONE', #3555, 6.499999999999988454 ) ;
#3351 = ORIENTED_EDGE ( 'NONE', *, *, #3310, .T. ) ;
#3352 = VERTEX_POINT ( 'NONE', #4813 ) ;
#3353 = CIRCLE ( 'NONE', #5083, 8.400000000000000355 ) ;
#3354 = DIRECTION ( 'NONE',  ( -1.000000000000000000, -0.000000000000000000, -0.000000000000000000 ) ) ;
#3355 = AXIS2_PLACEMENT_3D ( 'NONE', #87, #3850, #1284 ) ;
#3356 = ORIENTED_EDGE ( 'NONE', *, *, #3681, .F. ) ;
#3357 = VECTOR ( 'NONE', #3903, 999.9999999999998863 ) ;
#3358 = VECTOR ( 'NONE', #995, 1000.000000000000000 ) ;
#3359 = EDGE_CURVE ( 'NONE', #1224, #3015, #921, .T. ) ;
#3360 = ORIENTED_EDGE ( 'NONE', *, *, #3277, .F. ) ;
#3361 = CARTESIAN_POINT ( 'NONE',  ( 0.000000000000000000, 0.000000000000000000, 0.000000000000000000 ) ) ;
#3362 = LINE ( 'NONE', #2910, #148 ) ;
#3363 = DIRECTION ( 'NONE',  ( -0.000000000000000000, -0.000000000000000000, 1.000000000000000000 ) ) ;
#3364 = CIRCLE ( 'NONE', #3793, 5.036000000000040444 ) ;
#3365 = CONTEXT_DEPENDENT_SHAPE_REPRESENTATION ( #2309, #1480 ) ;
#3366 = EDGE_CURVE ( 'NONE', #3420, #3747, #3209, .T. ) ;
#3367 = ORIENTED_EDGE ( 'NONE', *, *, #1109, .F. ) ;
#3368 =( GEOMETRIC_REPRESENTATION_CONTEXT ( 3 ) GLOBAL_UNCERTAINTY_ASSIGNED_CONTEXT ( ( #2042 ) ) GLOBAL_UNIT_ASSIGNED_CONTEXT ( ( #4102, #707, #1168 ) ) REPRESENTATION_CONTEXT ( 'NONE', 'WORKASPACE' ) );
#3369 = CARTESIAN_POINT ( 'NONE',  ( 0.000000000000000000, -5.839897972853064445, 4.770489558936219510E-15 ) ) ;
#3370 = ORIENTED_EDGE ( 'NONE', *, *, #167, .F. ) ;
#3371 = CARTESIAN_POINT ( 'NONE',  ( 0.000000000000000000, 820.0000000000001137, 6.500000000000000000 ) ) ;
#3372 =( NAMED_UNIT ( * ) PLANE_ANGLE_UNIT ( ) SI_UNIT ( $, .RADIAN. ) );
#3373 = DIRECTION ( 'NONE',  ( -0.8191520442889902442, 0.000000000000000000, -0.5735764363510483799 ) ) ;
#3374 = CARTESIAN_POINT ( 'NONE',  ( 74.99999999999998579, 557.4999999999997726, 50.00000000000002132 ) ) ;
#3375 =( NAMED_UNIT ( * ) PLANE_ANGLE_UNIT ( ) SI_UNIT ( $, .RADIAN. ) );
#3376 = ADVANCED_FACE ( 'NONE', ( #4413 ), #4023, .F. ) ;
#3377 = ORIENTED_EDGE ( 'NONE', *, *, #2485, .T. ) ;
#3378 = TOROIDAL_SURFACE ( 'NONE', #321, 8.400000000000000355, 0.5999999999999999778 ) ;
#3379 =( NAMED_UNIT ( * ) SI_UNIT ( $, .STERADIAN. ) SOLID_ANGLE_UNIT ( ) );
#3380=STYLED_ITEM('',(#5405),#3645);
#3381 = FACE_OUTER_BOUND ( 'NONE', #5315, .T. ) ;
#3382 = CARTESIAN_POINT ( 'NONE',  ( 1.566316456955013869, -10.05335742100714747, -9.380055053747698324 ) ) ;
#3383 = VERTEX_POINT ( 'NONE', #5263 ) ;
#3384 = ORIENTED_EDGE ( 'NONE', *, *, #4429, .F. ) ;
#3385 = VERTEX_POINT ( 'NONE', #3195 ) ;
#3386 = VECTOR ( 'NONE', #3596, 1000.000000000000000 ) ;
#3387 = LINE ( 'NONE', #3817, #1511 ) ;
#3388 = ADVANCED_FACE ( 'NONE', ( #2789, #4047 ), #4874, .T. ) ;
#3389 = VECTOR ( 'NONE', #4337, 1000.000000000000000 ) ;
#3390 = SURFACE_STYLE_USAGE ( .BOTH. , #4219 ) ;
#3391 = EDGE_CURVE ( 'NONE', #676, #1204, #5030, .T. ) ;
#3392 = EDGE_LOOP ( 'NONE', ( #5366, #3012, #2223, #5051 ) ) ;
#3393 = CARTESIAN_POINT ( 'NONE',  ( -8.038218111920156501E-16, -10.97743472985186486, -9.686084310752816506 ) ) ;
#3394 = CARTESIAN_POINT ( 'NONE',  ( 150.0000000000000000, 810.0000000000000000, 25.00000000000000000 ) ) ;
#3395 = CARTESIAN_POINT ( 'NONE',  ( -31.74999999999995737, 0.000000000000000000, 0.000000000000000000 ) ) ;
#3396 = AXIS2_PLACEMENT_3D ( 'NONE', #4361, #950, #4284 ) ;
#3397 = AXIS2_PLACEMENT_3D ( 'NONE', #4992, #747, #2469 ) ;
#3398 = DIRECTION ( 'NONE',  ( 0.000000000000000000, 0.000000000000000000, -1.000000000000000000 ) ) ;
#3399 = CARTESIAN_POINT ( 'NONE',  ( 165.0000000000000000, 870.0000000000000000, 5.036000000000040444 ) ) ;
#3400 = DIRECTION ( 'NONE',  ( -1.000000000000000000, -0.000000000000000000, -0.000000000000000000 ) ) ;
#3401 = CARTESIAN_POINT ( 'NONE',  ( 150.0000000000000000, 870.0000000000000000, 5.999999999999894307 ) ) ;
#3402 = VERTEX_POINT ( 'NONE', #4961 ) ;
#3403 = DIRECTION ( 'NONE',  ( 0.000000000000000000, 1.000000000000000000, -1.039664082171044284E-15 ) ) ;
#3404 = APPLICATION_CONTEXT ( 'automotive_design' ) ;
#3405 = EDGE_LOOP ( 'NONE', ( #2135, #2258, #1389, #805 ) ) ;
#3406 = SURFACE_SIDE_STYLE ('',( #4630 ) ) ;
#3407 = CARTESIAN_POINT ( 'NONE',  ( 3.696995237865069228, 8.257843649639102779, -8.460795847313656637 ) ) ;
#3408 = CARTESIAN_POINT ( 'NONE',  ( 5.536779885055386430, -7.742692678355775904, -9.138972935415381471 ) ) ;
#3409 = CARTESIAN_POINT ( 'NONE',  ( 0.000000000000000000, 0.000000000000000000, -11.34441321561125626 ) ) ;
#3410 =( NAMED_UNIT ( * ) PLANE_ANGLE_UNIT ( ) SI_UNIT ( $, .RADIAN. ) );
#3411 = ADVANCED_FACE ( 'NONE', ( #1635 ), #1233, .T. ) ;
#3412 = ORIENTED_EDGE ( 'NONE', *, *, #3242, .F. ) ;
#3413 = ORIENTED_EDGE ( 'NONE', *, *, #2100, .F. ) ;
#3414 = SURFACE_STYLE_USAGE ( .BOTH. , #157 ) ;
#3415 = CARTESIAN_POINT ( 'NONE',  ( -30.00000000000000355, 10.00000000000000000, 30.00000000000000000 ) ) ;
#3416 = DIRECTION ( 'NONE',  ( 1.000000000000000000, 0.000000000000000000, 0.000000000000000000 ) ) ;
#3417 = AXIS2_PLACEMENT_3D ( 'NONE', #2603, #62, #4696 ) ;
#3418 = CARTESIAN_POINT ( 'NONE',  ( 8.758033615148258733, -5.911365213025767673, -9.525564194215363045 ) ) ;
#3419 = CARTESIAN_POINT ( 'NONE',  ( -121.7157287525381122, -20.00000000000000000, 121.7157287525380127 ) ) ;
#3420 = VERTEX_POINT ( 'NONE', #412 ) ;
#3421 = DIRECTION ( 'NONE',  ( 0.000000000000000000, -1.000000000000000000, 0.000000000000000000 ) ) ;
#3422 = CARTESIAN_POINT ( 'NONE',  ( 5.999999999999985789, 570.0000000000000000, 30.00000000000001066 ) ) ;
#3423 = ORIENTED_EDGE ( 'NONE', *, *, #4421, .T. ) ;
#3424 = CARTESIAN_POINT ( 'NONE',  ( -25.00000000000000000, 610.0000000000000000, 24.99999999999999645 ) ) ;
#3425 = EDGE_CURVE ( 'NONE', #871, #4239, #3728, .T. ) ;
#3426 = EDGE_LOOP ( 'NONE', ( #3604, #764, #2833, #4140 ) ) ;
#3427 = CARTESIAN_POINT ( 'NONE',  ( 11.99999999999999645, 0.000000000000000000, 9.000000000000000000 ) ) ;
#3428 = CARTESIAN_POINT ( 'NONE',  ( -4.500000000000002665, -7.794228634059946259, 0.000000000000000000 ) ) ;
#3429 = DIRECTION ( 'NONE',  ( 0.000000000000000000, 0.000000000000000000, -1.000000000000000000 ) ) ;
#3430 = EDGE_CURVE ( 'NONE', #1457, #1969, #984, .T. ) ;
#3431 = EDGE_CURVE ( 'NONE', #261, #2061, #581, .T. ) ;
#3432 = PRODUCT ( 'MAS-195', 'MAS-195', '', ( #2791 ) ) ;
#3433 = DIRECTION ( 'NONE',  ( 0.000000000000000000, 0.000000000000000000, -1.000000000000000000 ) ) ;
#3434 = AXIS2_PLACEMENT_3D ( 'NONE', #3870, #2642, #1374 ) ;
#3435 = ORIENTED_EDGE ( 'NONE', *, *, #4808, .T. ) ;
#3436 = FILL_AREA_STYLE_COLOUR ( '', #641 ) ;
#3437 = FACE_OUTER_BOUND ( 'NONE', #2618, .T. ) ;
#3438 = EDGE_CURVE ( 'NONE', #529, #870, #3561, .T. ) ;
#3439 = DIRECTION ( 'NONE',  ( 0.000000000000000000, 0.000000000000000000, 1.000000000000000000 ) ) ;
#3440 = AXIS2_PLACEMENT_3D ( 'NONE', #142, #4793, #1437 ) ;
#3441 = FACE_OUTER_BOUND ( 'NONE', #2158, .T. ) ;
#3442 = AXIS2_PLACEMENT_3D ( 'NONE', #4110, #3701, #3166 ) ;
#3443 = EDGE_LOOP ( 'NONE', ( #4424, #5015 ) ) ;
#3444 = DIRECTION ( 'NONE',  ( 2.081668171172168513E-16, 0.000000000000000000, -1.000000000000000000 ) ) ;
#3445 = CARTESIAN_POINT ( 'NONE',  ( 11.99999999999999645, 1.102182119232617714E-15, -9.000000000000000000 ) ) ;
#3446 = DIRECTION ( 'NONE',  ( 0.000000000000000000, 0.000000000000000000, -1.000000000000000000 ) ) ;
#3447 = EDGE_CURVE ( 'NONE', #2898, #4246, #3503, .T. ) ;
#3448 = CARTESIAN_POINT ( 'NONE',  ( 0.000000000000000000, 510.0000000000000000, -25.00000000000000000 ) ) ;
#3449 = EDGE_CURVE ( 'NONE', #2036, #3744, #1882, .T. ) ;
#3450 = VECTOR ( 'NONE', #960, 1000.000000000000000 ) ;
#3451 = CLOSED_SHELL ( 'NONE', ( #760, #4270, #4206, #2437, #372, #4774, #4100, #2897, #1300, #1527, #2218 ) ) ;
#3452 = ORIENTED_EDGE ( 'NONE', *, *, #1832, .T. ) ;
#3453 = CARTESIAN_POINT ( 'NONE',  ( 6.000000000000000000, 2.919948986426526005, -5.057500000000002771 ) ) ;
#3454 = EDGE_LOOP ( 'NONE', ( #3177, #867, #1490, #2028 ) ) ;
#3455 = DIRECTION ( 'NONE',  ( -0.000000000000000000, -1.000000000000000000, -0.000000000000000000 ) ) ;
#3456 = DIRECTION ( 'NONE',  ( 0.000000000000000000, -0.000000000000000000, 1.000000000000000000 ) ) ;
#3457 = DIRECTION ( 'NONE',  ( 9.251858538542972814E-17, 0.000000000000000000, -1.000000000000000000 ) ) ;
#3458 = CARTESIAN_POINT ( 'NONE',  ( 3.945874696944568161, -8.661172281173767473, -9.138600484129261403 ) ) ;
#3459 = CIRCLE ( 'NONE', #566, 5.036000000000040444 ) ;
#3460 = EDGE_CURVE ( 'NONE', #3262, #3466, #2812, .T. ) ;
#3461 = VECTOR ( 'NONE', #4707, 1000.000000000000000 ) ;
#3462 =( GEOMETRIC_REPRESENTATION_CONTEXT ( 3 ) GLOBAL_UNCERTAINTY_ASSIGNED_CONTEXT ( ( #2951 ) ) GLOBAL_UNIT_ASSIGNED_CONTEXT ( ( #669, #4801, #2832 ) ) REPRESENTATION_CONTEXT ( 'NONE', 'WORKASPACE' ) );
#3463 = DIRECTION ( 'NONE',  ( -1.000000000000000000, -0.000000000000000000, -0.000000000000000000 ) ) ;
#3464 = VECTOR ( 'NONE', #4290, 999.9999999999998863 ) ;
#3465 = VECTOR ( 'NONE', #972, 1000.000000000000000 ) ;
#3466 = VERTEX_POINT ( 'NONE', #5109 ) ;
#3467 = EDGE_CURVE ( 'NONE', #4833, #5330, #2296, .T. ) ;
#3468 = CARTESIAN_POINT ( 'NONE',  ( 6.000000000000000000, 0.000000000000000000, 0.000000000000000000 ) ) ;
#3469 = FACE_OUTER_BOUND ( 'NONE', #5077, .T. ) ;
#3470 = DIRECTION ( 'NONE',  ( 0.000000000000000000, 0.000000000000000000, -1.000000000000000000 ) ) ;
#3471 = AXIS2_PLACEMENT_3D ( 'NONE', #809, #1934, #4911 ) ;
#3472 = DIRECTION ( 'NONE',  ( 1.000000000000000000, 0.000000000000000000, 0.000000000000000000 ) ) ;
#3473 = FACE_OUTER_BOUND ( 'NONE', #398, .T. ) ;
#3474 = LINE ( 'NONE', #3059, #3465 ) ;
#3475 = VECTOR ( 'NONE', #714, 1000.000000000000000 ) ;
#3476 = DIRECTION ( 'NONE',  ( 0.000000000000000000, -1.000000000000000000, 0.000000000000000000 ) ) ;
#3477 = ORIENTED_EDGE ( 'NONE', *, *, #3460, .T. ) ;
#3478 = CYLINDRICAL_SURFACE ( 'NONE', #5117, 6.499999999999988454 ) ;
#3479 = SURFACE_SIDE_STYLE ('',( #1904 ) ) ;
#3480 = EDGE_CURVE ( 'NONE', #1452, #2957, #1068, .T. ) ;
#3481 = EDGE_CURVE ( 'NONE', #2978, #5042, #2715, .T. ) ;
#3482 = CARTESIAN_POINT ( 'NONE',  ( 1.453914506656636574, -9.552886913616360332, -0.5405968996909029656 ) ) ;
#3483 = CARTESIAN_POINT ( 'NONE',  ( -121.7157287525392917, 0.000000000000000000, -106.7157287525368332 ) ) ;
#3484 = CARTESIAN_POINT ( 'NONE',  ( 0.7181044661681106334, 9.977707038564833653, -0.8426663529491311699 ) ) ;
#3485 = DIRECTION ( 'NONE',  ( 1.000000000000000000, 0.000000000000000000, 0.000000000000000000 ) ) ;
#3486 = CARTESIAN_POINT ( 'NONE',  ( -6.499999999999988454, 450.0000000000000000, 25.00000000000000000 ) ) ;
#3487 = CARTESIAN_POINT ( 'NONE',  ( 5.284395884496541740, -7.341357458994639984, -0.03002505116510583924 ) ) ;
#3488 = VERTEX_POINT ( 'NONE', #2657 ) ;
#3489 = VERTEX_POINT ( 'NONE', #956 ) ;
#3490 = FACE_OUTER_BOUND ( 'NONE', #1372, .T. ) ;
#3491 = DIRECTION ( 'NONE',  ( -0.000000000000000000, -0.000000000000000000, 1.000000000000000000 ) ) ;
#3492 = DIRECTION ( 'NONE',  ( -0.000000000000000000, -0.000000000000000000, 1.000000000000000000 ) ) ;
#3493 = VERTEX_POINT ( 'NONE', #1047 ) ;
#3494 = ORIENTED_EDGE ( 'NONE', *, *, #859, .T. ) ;
#3495 = LINE ( 'NONE', #2647, #901 ) ;
#3496 = DIRECTION ( 'NONE',  ( -1.000000000000000000, 0.000000000000000000, -1.850371707708594316E-16 ) ) ;
#3497 = CARTESIAN_POINT ( 'NONE',  ( -9.000000000000000000, 3.464101615137751278, -8.667800885990208926 ) ) ;
#3498 = VERTEX_POINT ( 'NONE', #5135 ) ;
#3499 = DIRECTION ( 'NONE',  ( 0.000000000000000000, -0.000000000000000000, 1.000000000000000000 ) ) ;
#3500 = ORIENTED_EDGE ( 'NONE', *, *, #16, .T. ) ;
#3501 = DIRECTION ( 'NONE',  ( -0.000000000000000000, -1.000000000000000000, -0.000000000000000000 ) ) ;
#3502 = DIRECTION ( 'NONE',  ( -0.7071067811865291430, 8.659560562355159656E-17, -0.7071067811865660024 ) ) ;
#3503 = LINE ( 'NONE', #4684, #2422 ) ;
#3504 = DIRECTION ( 'NONE',  ( 0.9396926207859145341, 1.150791560227857665E-16, -0.3420201433256521151 ) ) ;
#3505 = DIRECTION ( 'NONE',  ( 0.000000000000000000, 0.000000000000000000, -1.000000000000000000 ) ) ;
#3506 = EDGE_CURVE ( 'NONE', #3498, #4363, #3296, .T. ) ;
#3507 = CARTESIAN_POINT ( 'NONE',  ( 0.000000000000000000, 810.0000000000000000, 6.499999999999999112 ) ) ;
#3508 = CARTESIAN_POINT ( 'NONE',  ( -24.99999999999999645, 810.0000000000000000, -25.00000000000000000 ) ) ;
#3509 = FILL_AREA_STYLE ('',( #990 ) ) ;
#3510 = ORIENTED_EDGE ( 'NONE', *, *, #564, .T. ) ;
#3511 = CARTESIAN_POINT ( 'NONE',  ( 165.0000000000000000, 870.0000000000000000, 0.000000000000000000 ) ) ;
#3512 = DIRECTION ( 'NONE',  ( -0.000000000000000000, -0.000000000000000000, 1.000000000000000000 ) ) ;
#3513 = DIRECTION ( 'NONE',  ( 0.000000000000000000, 0.000000000000000000, 1.000000000000000000 ) ) ;
#3514 = ADVANCED_FACE ( 'NONE', ( #4392 ), #112, .T. ) ;
#3515 = AXIS2_PLACEMENT_3D ( 'NONE', #1765, #3444, #1358 ) ;
#3516 = VERTEX_POINT ( 'NONE', #4766 ) ;
#3517 = VERTEX_POINT ( 'NONE', #3042 ) ;
#3518 = CARTESIAN_POINT ( 'NONE',  ( 150.0000000000000000, 10.00000000000000000, -150.0000000000000000 ) ) ;
#3519 = FILL_AREA_STYLE_COLOUR ( '', #4498 ) ;
#3520 = EDGE_CURVE ( 'NONE', #3851, #1518, #1017, .T. ) ;
#3521 = LINE ( 'NONE', #246, #1875 ) ;
#3522 = CARTESIAN_POINT ( 'NONE',  ( -74.99999999999998579, 582.4999999999997726, 29.99999999999999289 ) ) ;
#3523 = VECTOR ( 'NONE', #640, 1000.000000000000000 ) ;
#3524 = DIRECTION ( 'NONE',  ( 1.000000000000000000, 0.000000000000000000, 0.000000000000000000 ) ) ;
#3525 = AXIS2_PLACEMENT_3D ( 'NONE', #3468, #1373, #487 ) ;
#3526 = DIRECTION ( 'NONE',  ( 1.000000000000000000, 0.000000000000000000, 0.000000000000000000 ) ) ;
#3527 = CYLINDRICAL_SURFACE ( 'NONE', #5053, 6.499999999999988454 ) ;
#3528 = DIRECTION ( 'NONE',  ( 1.387778780781445676E-16, 0.000000000000000000, 1.000000000000000000 ) ) ;
#3529 = EDGE_CURVE ( 'NONE', #4754, #3040, #2244, .T. ) ;
#3530 = LINE ( 'NONE', #173, #4236 ) ;
#3531 = FACE_OUTER_BOUND ( 'NONE', #610, .T. ) ;
#3532 = AXIS2_PLACEMENT_3D ( 'NONE', #4955, #1563, #2064 ) ;
#3533 =( REPRESENTATION_RELATIONSHIP ('NONE','NONE', #4791, #1620 ) REPRESENTATION_RELATIONSHIP_WITH_TRANSFORMATION ( #5070 )SHAPE_REPRESENTATION_RELATIONSHIP( ) );
#3534 = VECTOR ( 'NONE', #1834, 999.9999999999998863 ) ;
#3535 = DIRECTION ( 'NONE',  ( 0.000000000000000000, 0.5000000000000012212, 0.8660254037844379305 ) ) ;
#3536 = DIRECTION ( 'NONE',  ( 0.000000000000000000, 0.000000000000000000, -1.000000000000000000 ) ) ;
#3537 = ORIENTED_EDGE ( 'NONE', *, *, #2341, .F. ) ;
#3538 = AXIS2_PLACEMENT_3D ( 'NONE', #2022, #1153, #2858 ) ;
#3539 = PRESENTATION_LAYER_ASSIGNMENT (  '', '', ( #2138 ) ) ;
#3540 = ADVANCED_FACE ( 'NONE', ( #2691 ), #4347, .F. ) ;
#3541 = ORIENTED_EDGE ( 'NONE', *, *, #2030, .T. ) ;
#3542 = EDGE_CURVE ( 'NONE', #5213, #3383, #5187, .T. ) ;
#3543 = CIRCLE ( 'NONE', #3808, 14.99999999999998579 ) ;
#3544 = ORIENTED_EDGE ( 'NONE', *, *, #4879, .F. ) ;
#3545 = LINE ( 'NONE', #2703, #472 ) ;
#3546=STYLED_ITEM('',(#5433),#3657);
#3547 = LINE ( 'NONE', #1394, #1211 ) ;
#3548 = PRODUCT_DEFINITION_SHAPE ( 'NONE', 'NONE',  #5389 ) ;
#3549 = ORIENTED_EDGE ( 'NONE', *, *, #5214, .T. ) ;
#3550 = DIRECTION ( 'NONE',  ( 0.000000000000000000, 0.4999999999999990008, -0.8660254037844392627 ) ) ;
#3551 = LINE ( 'NONE', #1379, #5384 ) ;
#3552 = CARTESIAN_POINT ( 'NONE',  ( 0.000000000000000000, 610.0000000000000000, -30.00000000000000355 ) ) ;
#3553 = CYLINDRICAL_SURFACE ( 'NONE', #4251, 6.499999999999983125 ) ;
#3554 = VECTOR ( 'NONE', #4468, 1000.000000000000000 ) ;
#3555 = AXIS2_PLACEMENT_3D ( 'NONE', #2952, #2193, #4245 ) ;
#3556 = VERTEX_POINT ( 'NONE', #4367 ) ;
#3557 = VECTOR ( 'NONE', #3736, 999.9999999999998863 ) ;
#3558 = CARTESIAN_POINT ( 'NONE',  ( -6.000000000000012434, 570.0000000000000000, 30.00000000000001066 ) ) ;
#3559 = EDGE_LOOP ( 'NONE', ( #303, #3977, #2046, #2960 ) ) ;
#3560 = SURFACE_SIDE_STYLE ('',( #190 ) ) ;
#3561 = LINE ( 'NONE', #1806, #3200 ) ;
#3562 = DIRECTION ( 'NONE',  ( 1.000000000000000000, 0.000000000000000000, 0.000000000000000000 ) ) ;
#3563 = CARTESIAN_POINT ( 'NONE',  ( 0.000000000000000000, 1.065442715258197248E-15, -8.400000000000000355 ) ) ;
#3564 = ORIENTED_EDGE ( 'NONE', *, *, #2955, .T. ) ;
#3565 = AXIS2_PLACEMENT_3D ( 'NONE', #3030, #3106, #617 ) ;
#3566 = PRODUCT_DEFINITION ( 'UNKNOWN', '', #3279, #5276 ) ;
#3567 = DIRECTION ( 'NONE',  ( 1.000000000000000000, 0.000000000000000000, 0.000000000000000000 ) ) ;
#3568 = DIRECTION ( 'NONE',  ( -2.081668171172168513E-16, 0.000000000000000000, 1.000000000000000000 ) ) ;
#3569 = VERTEX_POINT ( 'NONE', #1216 ) ;
#3570 =( LENGTH_UNIT ( ) NAMED_UNIT ( * ) SI_UNIT ( .MILLI., .METRE. ) );
#3571 = ORIENTED_EDGE ( 'NONE', *, *, #3366, .T. ) ;
#3572 = VERTEX_POINT ( 'NONE', #1932 ) ;
#3573 = VERTEX_POINT ( 'NONE', #4030 ) ;
#3574 = LINE ( 'NONE', #1056, #1940 ) ;
#3575 = DIRECTION ( 'NONE',  ( -0.000000000000000000, -0.000000000000000000, 1.000000000000000000 ) ) ;
#3576 = EDGE_CURVE ( 'NONE', #1861, #3047, #60, .T. ) ;
#3577 = EDGE_LOOP ( 'NONE', ( #2519, #1623, #903, #2286 ) ) ;
#3578 = VERTEX_POINT ( 'NONE', #5355 ) ;
#3579 = CARTESIAN_POINT ( 'NONE',  ( -9.058806161333684770, 5.230104175782638087, -9.269265075619308902 ) ) ;
#3580 = CARTESIAN_POINT ( 'NONE',  ( -9.562637692001347389, -5.457160213363115631, -9.698012095152312995 ) ) ;
#3581 = FACE_OUTER_BOUND ( 'NONE', #2925, .T. ) ;
#3582 = CARTESIAN_POINT ( 'NONE',  ( 0.000000000000000000, 510.0000000000000000, 25.00000000000000000 ) ) ;
#3583 = DIRECTION ( 'NONE',  ( 1.000000000000000000, 0.000000000000000000, 0.000000000000000000 ) ) ;
#3584 = VECTOR ( 'NONE', #3502, 1000.000000000000000 ) ;
#3585 = EDGE_LOOP ( 'NONE', ( #2610, #2456, #3856, #4020 ) ) ;
#3586 = DIRECTION ( 'NONE',  ( -1.000000000000000000, -0.000000000000000000, -0.000000000000000000 ) ) ;
#3587 = EDGE_LOOP ( 'NONE', ( #3902, #991 ) ) ;
#3588 = CARTESIAN_POINT ( 'NONE',  ( 0.000000000000000000, 5.839897972853065333, -6.938893903907228378E-15 ) ) ;
#3589 = FACE_OUTER_BOUND ( 'NONE', #265, .T. ) ;
#3590 = CARTESIAN_POINT ( 'NONE',  ( 9.000000000000000000, 5.196152422706629359, -8.935996291721334472 ) ) ;
#3591 = CARTESIAN_POINT ( 'NONE',  ( 0.000000000000000000, 0.000000000000000000, -11.97459999999999880 ) ) ;
#3592 = AXIS2_PLACEMENT_3D ( 'NONE', #5273, #3168, #694 ) ;
#3593 = ORIENTED_EDGE ( 'NONE', *, *, #1992, .F. ) ;
#3594 = ADVANCED_FACE ( 'NONE', ( #2384 ), #278, .T. ) ;
#3595 = CYLINDRICAL_SURFACE ( 'NONE', #2668, 6.000000000000001776 ) ;
#3596 = DIRECTION ( 'NONE',  ( -0.000000000000000000, -1.000000000000000000, -0.000000000000000000 ) ) ;
#3597 = ADVANCED_FACE ( 'NONE', ( #2822 ), #2446, .F. ) ;
#3598 = EDGE_LOOP ( 'NONE', ( #765, #3247, #4474, #3335 ) ) ;
#3599 = VECTOR ( 'NONE', #5354, 1000.000000000000000 ) ;
#3600 = VERTEX_POINT ( 'NONE', #2797 ) ;
#3601 = CARTESIAN_POINT ( 'NONE',  ( -9.506737344437272696, -5.488717364925931541, -9.686084310752812954 ) ) ;
#3602 = VERTEX_POINT ( 'NONE', #1605 ) ;
#3603 = CARTESIAN_POINT ( 'NONE',  ( -121.7157287525392917, -20.00000000000000000, -121.7157287525368332 ) ) ;
#3604 = ORIENTED_EDGE ( 'NONE', *, *, #458, .T. ) ;
#3605 = ORIENTED_EDGE ( 'NONE', *, *, #1420, .F. ) ;
#3606 = CARTESIAN_POINT ( 'NONE',  ( 0.000000000000000000, 0.000000000000000000, 0.000000000000000000 ) ) ;
#3607 = CARTESIAN_POINT ( 'NONE',  ( -3.712196824332475664, -8.249067009600855371, -8.964894084810355324 ) ) ;
#3608 = FACE_BOUND ( 'NONE', #5155, .T. ) ;
#3609 = CARTESIAN_POINT ( 'NONE',  ( 6.000000000000000000, 0.000000000000000000, 5.057500000000000107 ) ) ;
#3610 = EDGE_CURVE ( 'NONE', #1655, #4965, #467, .T. ) ;
#3611 = VERTEX_POINT ( 'NONE', #4420 ) ;
#3612 = ADVANCED_FACE ( 'NONE', ( #1908 ), #5274, .T. ) ;
#3613 = CARTESIAN_POINT ( 'NONE',  ( -139.9999999999999716, 870.0000000000000000, 0.000000000000000000 ) ) ;
#3614 = CIRCLE ( 'NONE', #3515, 6.499999999999983125 ) ;
#3615 = CARTESIAN_POINT ( 'NONE',  ( -6.332118058842091557, 7.287734290476352683, -9.190020220263406259 ) ) ;
#3616 = DIRECTION ( 'NONE',  ( 0.000000000000000000, -0.000000000000000000, 1.000000000000000000 ) ) ;
#3617 = ADVANCED_FACE ( 'NONE', ( #3589 ), #3653, .F. ) ;
#3618 = DIRECTION ( 'NONE',  ( -0.000000000000000000, -0.000000000000000000, -1.000000000000000000 ) ) ;
#3619 = AXIS2_PLACEMENT_3D ( 'NONE', #180, #4805, #4408 ) ;
#3620 = FACE_OUTER_BOUND ( 'NONE', #4070, .T. ) ;
#3621 = CARTESIAN_POINT ( 'NONE',  ( 9.000000000000000000, -5.196152422706636465, -8.935996291721336249 ) ) ;
#3622 = CIRCLE ( 'NONE', #1945, 5.999999999999950262 ) ;
#3623 = ORIENTED_EDGE ( 'NONE', *, *, #4201, .F. ) ;
#3624 = FILL_AREA_STYLE_COLOUR ( '', #141 ) ;
#3625 = ORIENTED_EDGE ( 'NONE', *, *, #1399, .F. ) ;
#3626 = AXIS2_PLACEMENT_3D ( 'NONE', #2782, #638, #3981 ) ;
#3627 = STYLED_ITEM ( 'NONE', ( #3748 ), #4286 ) ;
#3628 = MANIFOLD_SOLID_BREP ( 'Boss-Extrude1', #2665 ) ;
#3629 = ORIENTED_EDGE ( 'NONE', *, *, #5139, .F. ) ;
#3630 = DIRECTION ( 'NONE',  ( 1.000000000000000000, 0.000000000000000000, 0.000000000000000000 ) ) ;
#3631 = ORIENTED_EDGE ( 'NONE', *, *, #2968, .T. ) ;
#3632 = PLANE ( 'NONE',  #1170 ) ;
#3633 = AXIS2_PLACEMENT_3D ( 'NONE', #345, #4034, #2924 ) ;
#3634 = LINE ( 'NONE', #1982, #2222 ) ;
#3635 = AXIS2_PLACEMENT_3D ( 'NONE', #4693, #2704, #1864 ) ;
#3636 = ORIENTED_EDGE ( 'NONE', *, *, #435, .F. ) ;
#3637 = EDGE_CURVE ( 'NONE', #2065, #4833, #1577, .T. ) ;
#3638 = CIRCLE ( 'NONE', #5373, 6.000000000000006217 ) ;
#3639 = PRESENTATION_LAYER_ASSIGNMENT (  '', '', ( #1277 ) ) ;
#3640 = VERTEX_POINT ( 'NONE', #4502 ) ;
#3641 = CARTESIAN_POINT ( 'NONE',  ( 0.6000000000000033085, 1.028703311283776586E-15, -8.400000000000000355 ) ) ;
#3642 = CARTESIAN_POINT ( 'NONE',  ( -3.696995237864706851, -8.257843649639317718, -8.460795847314500406 ) ) ;
#3643 = DIRECTION ( 'NONE',  ( 1.000000000000000000, 0.000000000000000000, 0.000000000000000000 ) ) ;
#3644 = CARTESIAN_POINT ( 'NONE',  ( -150.0000000000000000, 870.0000000000000000, 0.000000000000000000 ) ) ;
#3645 = MANIFOLD_SOLID_BREP ( 'Boss-Extrude3', #1704 ) ;
#3646 =( NAMED_UNIT ( * ) PLANE_ANGLE_UNIT ( ) SI_UNIT ( $, .RADIAN. ) );
#3647 = AXIS2_PLACEMENT_3D ( 'NONE', #685, #775, #377 ) ;
#3648 = ORIENTED_EDGE ( 'NONE', *, *, #728, .T. ) ;
#3649 = ORIENTED_EDGE ( 'NONE', *, *, #3359, .F. ) ;
#3650 = CARTESIAN_POINT ( 'NONE',  ( -6.000000000000000888, 7.347880794884120722E-16, -25.03750572909317285 ) ) ;
#3651 = ORIENTED_EDGE ( 'NONE', *, *, #3126, .F. ) ;
#3652 = DIRECTION ( 'NONE',  ( -0.000000000000000000, -0.000000000000000000, 1.000000000000000000 ) ) ;
#3653 = PLANE ( 'NONE',  #1790 ) ;
#3654 = AXIS2_PLACEMENT_3D ( 'NONE', #4620, #4153, #891 ) ;
#3655 = DIRECTION ( 'NONE',  ( 1.000000000000000000, 0.000000000000000000, 0.000000000000000000 ) ) ;
#3656 = PLANE ( 'NONE',  #241 ) ;
#3657 = MANIFOLD_SOLID_BREP ( 'EndChamfer', #4567 ) ;
#3658 = ADVANCED_FACE ( 'NONE', ( #1690 ), #4550, .F. ) ;
#3659 = ORIENTED_EDGE ( 'NONE', *, *, #5060, .F. ) ;
#3660 = FACE_OUTER_BOUND ( 'NONE', #3405, .T. ) ;
#3661 = CARTESIAN_POINT ( 'NONE',  ( 8.999999999999996447, 4.330127018922190985, -8.787392856021021714 ) ) ;
#3662 = AXIS2_PLACEMENT_3D ( 'NONE', #3753, #9, #854 ) ;
#3663 = FILL_AREA_STYLE ('',( #3624 ) ) ;
#3664 = ORIENTED_EDGE ( 'NONE', *, *, #5292, .F. ) ;
#3665 = DIRECTION ( 'NONE',  ( 1.000000000000000000, 0.000000000000000000, 0.000000000000000000 ) ) ;
#3666 = ORIENTED_EDGE ( 'NONE', *, *, #4375, .T. ) ;
#3667 = EDGE_CURVE ( 'NONE', #2863, #1641, #1355, .T. ) ;
#3668 = ORIENTED_EDGE ( 'NONE', *, *, #1253, .T. ) ;
#3669 = CARTESIAN_POINT ( 'NONE',  ( 164.0360000000000014, 870.0000000000000000, 0.000000000000000000 ) ) ;
#3670 = CARTESIAN_POINT ( 'NONE',  ( -121.7157287525381122, -20.00000000000000000, 121.7157287525380127 ) ) ;
#3671 = DIRECTION ( 'NONE',  ( 1.000000000000000000, 0.000000000000000000, 0.000000000000000000 ) ) ;
#3672 = CARTESIAN_POINT ( 'NONE',  ( 6.000000000000000000, 7.347880794884119736E-16, -11.97459999999999880 ) ) ;
#3673 = ORIENTED_EDGE ( 'NONE', *, *, #1154, .F. ) ;
#3674 = CARTESIAN_POINT ( 'NONE',  ( -6.499999999999984901, 35.00000000000000000, -30.00000000000000711 ) ) ;
#3675 = ORIENTED_EDGE ( 'NONE', *, *, #365, .T. ) ;
#3676 = DIRECTION ( 'NONE',  ( 1.000000000000000000, 7.401486830834378251E-16, 0.000000000000000000 ) ) ;
#3677 = CARTESIAN_POINT ( 'NONE',  ( 12.00000000000000000, 0.000000000000000000, 0.000000000000000000 ) ) ;
#3678 = CARTESIAN_POINT ( 'NONE',  ( 6.000000000000000000, 2.919948986426526005, -5.057500000000002771 ) ) ;
#3679 = DIRECTION ( 'NONE',  ( 0.000000000000000000, -0.000000000000000000, 1.000000000000000000 ) ) ;
#3680 = VECTOR ( 'NONE', #3455, 1000.000000000000000 ) ;
#3681 = EDGE_CURVE ( 'NONE', #3270, #1603, #2239, .T. ) ;
#3682 = EDGE_LOOP ( 'NONE', ( #4410, #4783 ) ) ;
#3683 = CYLINDRICAL_SURFACE ( 'NONE', #3725, 6.499999999999983125 ) ;
#3684 = CARTESIAN_POINT ( 'NONE',  ( 9.000000000000001776, -4.330127018922196314, -8.787392856021023491 ) ) ;
#3685 = EDGE_LOOP ( 'NONE', ( #2684, #4617 ) ) ;
#3686 = ORIENTED_EDGE ( 'NONE', *, *, #611, .T. ) ;
#3687 = ORIENTED_EDGE ( 'NONE', *, *, #894, .F. ) ;
#3688 =( LENGTH_UNIT ( ) NAMED_UNIT ( * ) SI_UNIT ( .MILLI., .METRE. ) );
#3689 = CARTESIAN_POINT ( 'NONE',  ( -150.0000000000000000, 885.0000000000000000, -25.00000000000000000 ) ) ;
#3690 = ADVANCED_FACE ( 'NONE', ( #14 ), #415, .T. ) ;
#3691 = ORIENTED_EDGE ( 'NONE', *, *, #3838, .T. ) ;
#3692 = SURFACE_STYLE_FILL_AREA ( #1541 ) ;
#3693 = ORIENTED_EDGE ( 'NONE', *, *, #2144, .F. ) ;
#3694 = DIRECTION ( 'NONE',  ( 0.000000000000000000, 0.000000000000000000, -1.000000000000000000 ) ) ;
#3695 = CARTESIAN_POINT ( 'NONE',  ( -1.272360546691562622, -9.657707141274665119, -9.220334578152071359 ) ) ;
#3696 = CARTESIAN_POINT ( 'NONE',  ( 9.497968775322179980, 4.580952057516532783, -9.518120616476199558 ) ) ;
#3697 = DIRECTION ( 'NONE',  ( 0.000000000000000000, -0.000000000000000000, 1.000000000000000000 ) ) ;
#3698 = APPLICATION_PROTOCOL_DEFINITION ( 'draft international standard', 'automotive_design', 1998, #5230 ) ;
#3699 = EDGE_CURVE ( 'NONE', #3733, #81, #1440, .T. ) ;
#3700 = EDGE_CURVE ( 'NONE', #1225, #2529, #2617, .T. ) ;
#3701 = DIRECTION ( 'NONE',  ( -0.5000000000000004441, -0.8660254037844384856, 0.000000000000000000 ) ) ;
#3702 = ORIENTED_EDGE ( 'NONE', *, *, #3872, .T. ) ;
#3703 = CARTESIAN_POINT ( 'NONE',  ( 137.5000000000000000, 870.0000000000000000, -6.000000000000006217 ) ) ;
#3704 = DIRECTION ( 'NONE',  ( 0.000000000000000000, 0.000000000000000000, -1.000000000000000000 ) ) ;
#3705 = CYLINDRICAL_SURFACE ( 'NONE', #3471, 6.000000000000006217 ) ;
#3706 = SHAPE_REPRESENTATION ( 'base', ( #4154 ), #3368 ) ;
#3707 = VECTOR ( 'NONE', #3080, 1000.000000000000000 ) ;
#3708 = EDGE_CURVE ( 'NONE', #4571, #3402, #2551, .T. ) ;
#3709 = ORIENTED_EDGE ( 'NONE', *, *, #1241, .T. ) ;
#3710 = ORIENTED_EDGE ( 'NONE', *, *, #1362, .F. ) ;
#3711 = CARTESIAN_POINT ( 'NONE',  ( 0.000000000000000000, 0.000000000000000000, -10.20000000000000107 ) ) ;
#3712 = CARTESIAN_POINT ( 'NONE',  ( -7.500000000000000000, 6.062177826491067734, -8.667800885990208926 ) ) ;
#3713 = EDGE_LOOP ( 'NONE', ( #558, #816 ) ) ;
#3714 = EDGE_LOOP ( 'NONE', ( #4722, #3072, #82, #2259 ) ) ;
#3715 = VECTOR ( 'NONE', #103, 1000.000000000000000 ) ;
#3716 = EDGE_LOOP ( 'NONE', ( #4373, #3110, #782, #2901 ) ) ;
#3717 = AXIS2_PLACEMENT_3D ( 'NONE', #3255, #2820, #306 ) ;
#3718 = CARTESIAN_POINT ( 'NONE',  ( -1.676835913137321903E-15, 35.00000000000000000, 30.00000000000000711 ) ) ;
#3719 = ORIENTED_EDGE ( 'NONE', *, *, #110, .F. ) ;
#3720 = FILL_AREA_STYLE_COLOUR ( '', #751 ) ;
#3721 = VECTOR ( 'NONE', #4145, 1000.000000000000000 ) ;
#3722 = EDGE_CURVE ( 'NONE', #3218, #4512, #2575, .T. ) ;
#3723 = ADVANCED_FACE ( 'NONE', ( #3853, #2261, #2648, #1766, #1870, #4697 ), #3113, .F. ) ;
#3724 = ORIENTED_EDGE ( 'NONE', *, *, #5316, .T. ) ;
#3725 = AXIS2_PLACEMENT_3D ( 'NONE', #2450, #4976, #2800 ) ;
#3726 = CARTESIAN_POINT ( 'NONE',  ( 139.9999999999999716, 870.0000000000000000, 0.000000000000000000 ) ) ;
#3727 = CARTESIAN_POINT ( 'NONE',  ( -7.784221022415209745, 5.898082742690295532, -8.707326526324866478 ) ) ;
#3728 = LINE ( 'NONE', #4735, #3464 ) ;
#3729 = CARTESIAN_POINT ( 'NONE',  ( 5.287803175666998534, -7.339390258519116195, -8.964894084810353547 ) ) ;
#3730 = AXIS2_PLACEMENT_3D ( 'NONE', #441, #3777, #3343 ) ;
#3731 = AXIS2_PLACEMENT_3D ( 'NONE', #1009, #3934, #545 ) ;
#3732 = PRESENTATION_STYLE_ASSIGNMENT (( #3414 ) ) ;
#3733 = VERTEX_POINT ( 'NONE', #3445 ) ;
#3734 = CARTESIAN_POINT ( 'NONE',  ( -6.499999999999984901, 35.00000000000000000, 25.00000000000000000 ) ) ;
#3735 = CARTESIAN_POINT ( 'NONE',  ( 0.000000000000000000, 390.0000000000000000, 25.00000000000000000 ) ) ;
#3736 = DIRECTION ( 'NONE',  ( 0.000000000000000000, -0.5000000000000012212, -0.8660254037844380415 ) ) ;
#3737 = VECTOR ( 'NONE', #4309, 1000.000000000000000 ) ;
#3738 = VERTEX_POINT ( 'NONE', #1431 ) ;
#3739 = EDGE_LOOP ( 'NONE', ( #1867, #4810 ) ) ;
#3740 = DIRECTION ( 'NONE',  ( 0.000000000000000000, 0.000000000000000000, -1.000000000000000000 ) ) ;
#3741 = DIRECTION ( 'NONE',  ( 0.000000000000000000, 0.000000000000000000, -1.000000000000000000 ) ) ;
#3742 = EDGE_LOOP ( 'NONE', ( #3675, #3229, #4177 ) ) ;
#3743 = AXIS2_PLACEMENT_3D ( 'NONE', #2741, #3888, #1808 ) ;
#3744 = VERTEX_POINT ( 'NONE', #570 ) ;
#3745 = CIRCLE ( 'NONE', #1446, 5.035999999999999588 ) ;
#3746 = DIRECTION ( 'NONE',  ( -0.000000000000000000, -0.000000000000000000, 1.000000000000000000 ) ) ;
#3747 = VERTEX_POINT ( 'NONE', #4724 ) ;
#3748 = PRESENTATION_STYLE_ASSIGNMENT (( #3390 ) ) ;
#3749 = ORIENTED_EDGE ( 'NONE', *, *, #3900, .T. ) ;
#3750 = LINE ( 'NONE', #434, #3789 ) ;
#3751 = EDGE_CURVE ( 'NONE', #3154, #3895, #3035, .T. ) ;
#3752 = CARTESIAN_POINT ( 'NONE',  ( -7.950863337915141216, 6.367515845290393273, -9.383905213720927563 ) ) ;
#3753 = CARTESIAN_POINT ( 'NONE',  ( -150.0000000000000284, 10.00000000000000000, 149.9999999999999147 ) ) ;
#3754 = ITEM_DEFINED_TRANSFORMATION ( 'NONE', 'NONE', #1352,  #4154 ) ;
#3755 = DIRECTION ( 'NONE',  ( 0.000000000000000000, 0.000000000000000000, 1.000000000000000000 ) ) ;
#3756 =( NAMED_UNIT ( * ) PLANE_ANGLE_UNIT ( ) SI_UNIT ( $, .RADIAN. ) );
#3757 = DIRECTION ( 'NONE',  ( -0.000000000000000000, -0.000000000000000000, 1.000000000000000000 ) ) ;
#3758 = DIRECTION ( 'NONE',  ( 0.000000000000000000, 0.000000000000000000, 1.000000000000000000 ) ) ;
#3759 =( LENGTH_UNIT ( ) NAMED_UNIT ( * ) SI_UNIT ( .MILLI., .METRE. ) );
#3760 = ORIENTED_EDGE ( 'NONE', *, *, #2091, .T. ) ;
#3761 = FACE_OUTER_BOUND ( 'NONE', #1200, .T. ) ;
#3762 = UNCERTAINTY_MEASURE_WITH_UNIT (LENGTH_MEASURE( 1.000000000000000082E-05 ), #4296, 'distance_accuracy_value', 'NONE');
#3763 = CARTESIAN_POINT ( 'NONE',  ( -8.038218111920156501E-16, -10.97743472985186486, -9.686084310752816506 ) ) ;
#3764 = ORIENTED_EDGE ( 'NONE', *, *, #3783, .F. ) ;
#3765 = VERTEX_POINT ( 'NONE', #4676 ) ;
#3766 = EDGE_CURVE ( 'NONE', #539, #3274, #5293, .T. ) ;
#3767 = EDGE_CURVE ( 'NONE', #5330, #3942, #3551, .T. ) ;
#3768 = CARTESIAN_POINT ( 'NONE',  ( 25.00000000000000000, 810.0000000000000000, 25.00000000000000711 ) ) ;
#3769 = ORIENTED_EDGE ( 'NONE', *, *, #2913, .T. ) ;
#3770 = SURFACE_STYLE_USAGE ( .BOTH. , #4123 ) ;
#3771 = VERTEX_POINT ( 'NONE', #2234 ) ;
#3772 = DIRECTION ( 'NONE',  ( 0.000000000000000000, 0.000000000000000000, -1.000000000000000000 ) ) ;
#3773 = CARTESIAN_POINT ( 'NONE',  ( -7.727639453308069228, 5.930750126845744319, -9.220334578152877825 ) ) ;
#3774 = DIRECTION ( 'NONE',  ( -0.000000000000000000, 1.000000000000000000, -0.000000000000000000 ) ) ;
#3775 = DIRECTION ( 'NONE',  ( -0.000000000000000000, -0.000000000000000000, 1.000000000000000000 ) ) ;
#3776 = FACE_OUTER_BOUND ( 'NONE', #1137, .T. ) ;
#3777 = DIRECTION ( 'NONE',  ( -0.000000000000000000, 0.000000000000000000, 1.000000000000000000 ) ) ;
#3778 = ADVANCED_FACE ( 'NONE', ( #163 ), #3931, .F. ) ;
#3779 = CARTESIAN_POINT ( 'NONE',  ( -9.000000000002474465, -4.659239318103709060, -9.367154206100524405 ) ) ;
#3780 = MANIFOLD_SOLID_BREP ( 'M12 Clearance Hole1', #3096 ) ;
#3781 = ORIENTED_EDGE ( 'NONE', *, *, #4878, .F. ) ;
#3782 = ADVANCED_FACE ( 'NONE', ( #2604 ), #3957, .T. ) ;
#3783 = EDGE_CURVE ( 'NONE', #3040, #2114, #3299, .T. ) ;
#3784 = ORIENTED_EDGE ( 'NONE', *, *, #3425, .T. ) ;
#3785 = DIRECTION ( 'NONE',  ( 0.000000000000000000, 0.000000000000000000, 1.000000000000000000 ) ) ;
#3786 = CARTESIAN_POINT ( 'NONE',  ( 9.000000000000000000, 2.225465271616588581, -0.2256151218434061245 ) ) ;
#3787 = EDGE_LOOP ( 'NONE', ( #3377, #3033, #5010, #4835 ) ) ;
#3788 = ORIENTED_EDGE ( 'NONE', *, *, #2076, .T. ) ;
#3789 = VECTOR ( 'NONE', #2488, 1000.000000000000000 ) ;
#3790 = DIRECTION ( 'NONE',  ( 0.000000000000000000, -1.000000000000000000, 0.000000000000000000 ) ) ;
#3791 = CIRCLE ( 'NONE', #2571, 12.07201791628681420 ) ;
#3792 = ORIENTED_EDGE ( 'NONE', *, *, #4019, .T. ) ;
#3793 = AXIS2_PLACEMENT_3D ( 'NONE', #2197, #2147, #5089 ) ;
#3794 = ORIENTED_EDGE ( 'NONE', *, *, #1670, .F. ) ;
#3795 = DIRECTION ( 'NONE',  ( 0.000000000000000000, 0.000000000000000000, -1.000000000000000000 ) ) ;
#3796 = CARTESIAN_POINT ( 'NONE',  ( 150.0000000000000000, 810.0000000000000000, 25.00000000000000000 ) ) ;
#3797 = CARTESIAN_POINT ( 'NONE',  ( -6.048361762532168839, -6.900281553659082689, -0.1192015822679202974 ) ) ;
#3798 = AXIS2_PLACEMENT_3D ( 'NONE', #3409, #4615, #454 ) ;
#3799 = EDGE_CURVE ( 'NONE', #4209, #2382, #1796, .T. ) ;
#3800 = AXIS2_PLACEMENT_3D ( 'NONE', #5163, #5192, #3973 ) ;
#3801 = AXIS2_PLACEMENT_3D ( 'NONE', #1895, #3575, #2785 ) ;
#3802 = CARTESIAN_POINT ( 'NONE',  ( -9.000000000000000000, 0.9001646245238090760, -0.03631462189738247914 ) ) ;
#3803 = LINE ( 'NONE', #2550, #4513 ) ;
#3804 = DIRECTION ( 'NONE',  ( -0.000000000000000000, 1.000000000000000000, -0.000000000000000000 ) ) ;
#3805 = PLANE ( 'NONE',  #4593 ) ;
#3806 = AXIS2_PLACEMENT_3D ( 'NONE', #4652, #2080, #924 ) ;
#3807 = MECHANICAL_DESIGN_GEOMETRIC_PRESENTATION_REPRESENTATION (  '', ( #491 ), #3288 ) ;
#3808 = AXIS2_PLACEMENT_3D ( 'NONE', #1006, #5178, #1432 ) ;
#3809 = LINE ( 'NONE', #526, #962 ) ;
#3810 = COLOUR_RGB ( '',0.8941176470588234615, 0.8941176470588234615, 0.8941176470588234615 ) ;
#3811 = CARTESIAN_POINT ( 'NONE',  ( 25.00000000000000000, 810.0000000000000000, 25.00000000000000711 ) ) ;
#3812 = UNCERTAINTY_MEASURE_WITH_UNIT (LENGTH_MEASURE( 1.000000000000000082E-05 ), #3759, 'distance_accuracy_value', 'NONE');
#3813 = CARTESIAN_POINT ( 'NONE',  ( 7.921880722261732011, -6.383959649155164229, -9.379910571084325355 ) ) ;
#3814 = EDGE_CURVE ( 'NONE', #508, #2478, #3474, .T. ) ;
#3815 = ORIENTED_EDGE ( 'NONE', *, *, #531, .F. ) ;
#3816 = AXIS2_PLACEMENT_3D ( 'NONE', #541, #3878, #133 ) ;
#3817 = CARTESIAN_POINT ( 'NONE',  ( -25.00000000000000000, 10.00000000000000000, 24.99999999999999645 ) ) ;
#3818 = AXIS2_PLACEMENT_3D ( 'NONE', #5111, #3045, #3017 ) ;
#3819 =( LENGTH_UNIT ( ) NAMED_UNIT ( * ) SI_UNIT ( .MILLI., .METRE. ) );
#3820 = VECTOR ( 'NONE', #4234, 1000.000000000000000 ) ;
#3821 = VERTEX_POINT ( 'NONE', #684 ) ;
#3822 = CARTESIAN_POINT ( 'NONE',  ( -12.07201791628681598, 1.478395810043015094E-15, -11.07201791628681775 ) ) ;
#3823 = FACE_BOUND ( 'NONE', #3713, .T. ) ;
#3824 = CARTESIAN_POINT ( 'NONE',  ( -1.676835913137321903E-15, 35.00000000000000000, 30.00000000000000711 ) ) ;
#3825 = DIRECTION ( 'NONE',  ( 0.000000000000000000, 0.000000000000000000, 1.000000000000000000 ) ) ;
#3826 = AXIS2_PLACEMENT_3D ( 'NONE', #1454, #2199, #3513 ) ;
#3827 = ADVANCED_FACE ( 'NONE', ( #4079 ), #4841, .T. ) ;
#3828 = CARTESIAN_POINT ( 'NONE',  ( -9.000000000000000000, 2.225465271616585472, -0.2256151218434065964 ) ) ;
#3829 = FACE_OUTER_BOUND ( 'NONE', #3996, .T. ) ;
#3830 = ADVANCED_FACE ( 'NONE', ( #1545 ), #642, .F. ) ;
#3831 = DIRECTION ( 'NONE',  ( 0.000000000000000000, 0.000000000000000000, 1.000000000000000000 ) ) ;
#3832 = EDGE_LOOP ( 'NONE', ( #1150, #2783, #1930, #5107 ) ) ;
#3833 = CARTESIAN_POINT ( 'NONE',  ( -8.999999999999998224, -1.854975783832116143, -9.019265669392103391 ) ) ;
#3834 = LINE ( 'NONE', #2583, #1836 ) ;
#3835 = CARTESIAN_POINT ( 'NONE',  ( 3.954162315725771482, 8.656288888417748240, -9.137374534098841039 ) ) ;
#3836 = PLANE ( 'NONE',  #3818 ) ;
#3837 = ORIENTED_EDGE ( 'NONE', *, *, #5105, .T. ) ;
#3838 = EDGE_CURVE ( 'NONE', #791, #4561, #1201, .T. ) ;
#3839 = DIRECTION ( 'NONE',  ( 1.000000000000000000, 0.000000000000000000, 0.000000000000000000 ) ) ;
#3840 =( NAMED_UNIT ( * ) SI_UNIT ( $, .STERADIAN. ) SOLID_ANGLE_UNIT ( ) );
#3841 = EDGE_CURVE ( 'NONE', #3573, #813, #4494, .T. ) ;
#3842 = VERTEX_POINT ( 'NONE', #2816 ) ;
#3843 = FACE_OUTER_BOUND ( 'NONE', #2122, .T. ) ;
#3844 = VECTOR ( 'NONE', #5217, 1000.000000000000000 ) ;
#3845 = ORIENTED_EDGE ( 'NONE', *, *, #4897, .T. ) ;
#3846 = DIRECTION ( 'NONE',  ( 0.000000000000000000, 0.000000000000000000, -1.000000000000000000 ) ) ;
#3847 = DIRECTION ( 'NONE',  ( 1.000000000000000000, 0.000000000000000000, 0.000000000000000000 ) ) ;
#3848 = ITEM_DEFINED_TRANSFORMATION ( 'NONE', 'NONE', #2758,  #4154 ) ;
#3849 = PRESENTATION_LAYER_ASSIGNMENT (  '', '', ( #1750 ) ) ;
#3850 = DIRECTION ( 'NONE',  ( 0.000000000000000000, 0.000000000000000000, 1.000000000000000000 ) ) ;
#3851 = VERTEX_POINT ( 'NONE', #5262 ) ;
#3852 = CARTESIAN_POINT ( 'NONE',  ( 9.497981232281496489, -4.582241663078509220, -9.518359232022067573 ) ) ;
#3853 = FACE_BOUND ( 'NONE', #3587, .T. ) ;
#3854 = CARTESIAN_POINT ( 'NONE',  ( 0.000000000000000000, 0.000000000000000000, -10.20000000000000107 ) ) ;
#3855 = ADVANCED_FACE ( 'NONE', ( #3159 ), #774, .T. ) ;
#3856 = ORIENTED_EDGE ( 'NONE', *, *, #4038, .T. ) ;
#3857 = CARTESIAN_POINT ( 'NONE',  ( -9.000000000000000000, -0.9100846702111624609, -8.964906921228866565 ) ) ;
#3858 =( LENGTH_UNIT ( ) NAMED_UNIT ( * ) SI_UNIT ( .MILLI., .METRE. ) );
#3859 = ORIENTED_EDGE ( 'NONE', *, *, #2543, .T. ) ;
#3860 = LINE ( 'NONE', #111, #3680 ) ;
#3861 = CARTESIAN_POINT ( 'NONE',  ( 4.500000000000003553, 7.794228634059947147, 0.000000000000000000 ) ) ;
#3862 = DIRECTION ( 'NONE',  ( -1.000000000000000000, 0.000000000000000000, 0.000000000000000000 ) ) ;
#3863 = SHAPE_REPRESENTATION ( 'main roller', ( #4154 ), #755 ) ;
#3864 = FACE_OUTER_BOUND ( 'NONE', #615, .T. ) ;
#3865 = ADVANCED_FACE ( 'NONE', ( #4022 ), #738, .T. ) ;
#3866 = CYLINDRICAL_SURFACE ( 'NONE', #5364, 6.499999999999983125 ) ;
#3867 = VECTOR ( 'NONE', #3224, 1000.000000000000000 ) ;
#3868 = ORIENTED_EDGE ( 'NONE', *, *, #1980, .F. ) ;
#3869 = CARTESIAN_POINT ( 'NONE',  ( -165.0000000000000000, 870.0000000000000000, 5.036000000000040444 ) ) ;
#3870 = CARTESIAN_POINT ( 'NONE',  ( -25.00000000000000000, 610.0000000000000000, 24.99999999999999645 ) ) ;
#3871 = LINE ( 'NONE', #969, #1890 ) ;
#3872 = EDGE_CURVE ( 'NONE', #4147, #819, #1061, .T. ) ;
#3873 = VECTOR ( 'NONE', #4355, 1000.000000000000000 ) ;
#3874 = EDGE_CURVE ( 'NONE', #3466, #2534, #1424, .T. ) ;
#3875 = PLANE ( 'NONE',  #295 ) ;
#3876 = ORIENTED_EDGE ( 'NONE', *, *, #1417, .T. ) ;
#3877 = CARTESIAN_POINT ( 'NONE',  ( 150.0000000000000000, 0.000000000000000000, -150.0000000000000000 ) ) ;
#3878 = DIRECTION ( 'NONE',  ( -0.000000000000000000, -0.000000000000000000, 1.000000000000000000 ) ) ;
#3879 = CARTESIAN_POINT ( 'NONE',  ( 12.07201791628681598, 0.000000000000000000, -11.07201791628681775 ) ) ;
#3880 = CARTESIAN_POINT ( 'NONE',  ( -139.9999999999999716, 885.0000000000000000, -25.00000000000000000 ) ) ;
#3881 = AXIS2_PLACEMENT_3D ( 'NONE', #4688, #1709, #4594 ) ;
#3882 = CIRCLE ( 'NONE', #2941, 14.99999999999998579 ) ;
#3883 = CARTESIAN_POINT ( 'NONE',  ( 9.000000000000000000, -0.9015406389697717682, 1.338312056661794536E-15 ) ) ;
#3884 = ORIENTED_EDGE ( 'NONE', *, *, #3766, .T. ) ;
#3885 = DIRECTION ( 'NONE',  ( 1.000000000000000000, 0.000000000000000000, 0.000000000000000000 ) ) ;
#3886 = CARTESIAN_POINT ( 'NONE',  ( 2.569563281917983666, 8.908766792898136444, -0.2264046624879769432 ) ) ;
#3887 = CARTESIAN_POINT ( 'NONE',  ( 0.000000000000000000, 570.0000000000000000, 25.00000000000000000 ) ) ;
#3888 = DIRECTION ( 'NONE',  ( -1.000000000000000000, -0.000000000000000000, -0.000000000000000000 ) ) ;
#3889 = AXIS2_PLACEMENT_3D ( 'NONE', #985, #1807, #2297 ) ;
#3890 = CIRCLE ( 'NONE', #4575, 6.499999999999988454 ) ;
#3891 = PRESENTATION_LAYER_ASSIGNMENT (  '', '', ( #5019 ) ) ;
#3892 = LINE ( 'NONE', #2140, #2219 ) ;
#3893 = COLOUR_RGB ( '',1.000000000000000000, 0.9490196078431372140, 0.9098039215686274384 ) ;
#3894 = AXIS2_PLACEMENT_3D ( 'NONE', #5222, #3568, #5164 ) ;
#3895 = VERTEX_POINT ( 'NONE', #4900 ) ;
#3896 = FILL_AREA_STYLE ('',( #3436 ) ) ;
#3897 = FACE_OUTER_BOUND ( 'NONE', #2106, .T. ) ;
#3898 = DIRECTION ( 'NONE',  ( 1.000000000000000000, 0.000000000000000000, 0.000000000000000000 ) ) ;
#3899 = AXIS2_PLACEMENT_3D ( 'NONE', #5189, #225, #3916 ) ;
#3900 = EDGE_CURVE ( 'NONE', #701, #508, #1901, .T. ) ;
#3901 = EDGE_LOOP ( 'NONE', ( #177, #1483, #1770, #1678 ) ) ;
#3902 = ORIENTED_EDGE ( 'NONE', *, *, #5027, .T. ) ;
#3903 = DIRECTION ( 'NONE',  ( -0.7071067811865577868, 8.659560562354808366E-17, -0.7071067811865373587 ) ) ;
#3904 = CARTESIAN_POINT ( 'NONE',  ( -150.0000000000000284, 10.00000000000000000, 149.9999999999999147 ) ) ;
#3905 = CIRCLE ( 'NONE', #1291, 5.999999999999996447 ) ;
#3906 = CARTESIAN_POINT ( 'NONE',  ( -9.000000000000000000, -2.405731887095257756E-15, -8.419403919045802098 ) ) ;
#3907 = ORIENTED_EDGE ( 'NONE', *, *, #233, .T. ) ;
#3908 = LINE ( 'NONE', #2206, #2430 ) ;
#3909 = CARTESIAN_POINT ( 'NONE',  ( 0.000000000000000000, 0.000000000000000000, 0.000000000000000000 ) ) ;
#3910 = ADVANCED_FACE ( 'NONE', ( #5324 ), #1568, .T. ) ;
#3911 = ORIENTED_EDGE ( 'NONE', *, *, #4247, .T. ) ;
#3912 = LINE ( 'NONE', #3963, #1078 ) ;
#3913 = DIRECTION ( 'NONE',  ( 0.000000000000000000, 0.000000000000000000, 1.000000000000000000 ) ) ;
#3914 = DIRECTION ( 'NONE',  ( 0.000000000000000000, -0.4999999999999991118, 0.8660254037844390407 ) ) ;
#3915 = LINE ( 'NONE', #1069, #3461 ) ;
#3916 = DIRECTION ( 'NONE',  ( 0.000000000000000000, 0.000000000000000000, 1.000000000000000000 ) ) ;
#3917 = ORIENTED_EDGE ( 'NONE', *, *, #98, .T. ) ;
#3918 = CARTESIAN_POINT ( 'NONE',  ( -165.0000000000000000, 870.0000000000000000, -5.036000000000040444 ) ) ;
#3919 = CARTESIAN_POINT ( 'NONE',  ( 4.500000000000000000, 7.794228634059944483, -8.419403919045800322 ) ) ;
#3920 = VERTEX_POINT ( 'NONE', #1281 ) ;
#3921 = EDGE_CURVE ( 'NONE', #3821, #1397, #4179, .T. ) ;
#3922 = ORIENTED_EDGE ( 'NONE', *, *, #4856, .F. ) ;
#3923 = ADVANCED_FACE ( 'NONE', ( #1659 ), #1072, .F. ) ;
#3924 = ORIENTED_EDGE ( 'NONE', *, *, #211, .F. ) ;
#3925 = CARTESIAN_POINT ( 'NONE',  ( 150.0000000000000000, 870.0000000000000000, -5.999999999999894307 ) ) ;
#3926 = CARTESIAN_POINT ( 'NONE',  ( -6.499999999999988454, 510.0000000000000000, -25.00000000000000000 ) ) ;
#3927 = EDGE_CURVE ( 'NONE', #1447, #3640, #1206, .T. ) ;
#3928 = ORIENTED_EDGE ( 'NONE', *, *, #1667, .F. ) ;
#3929 = ORIENTED_EDGE ( 'NONE', *, *, #167, .T. ) ;
#3930 = DIRECTION ( 'NONE',  ( 0.000000000000000000, 0.000000000000000000, 1.000000000000000000 ) ) ;
#3931 = PLANE ( 'NONE',  #3026 ) ;
#3932 = CARTESIAN_POINT ( 'NONE',  ( -25.00000000000000000, 610.0000000000000000, 24.99999999999999645 ) ) ;
#3933 = CARTESIAN_POINT ( 'NONE',  ( -137.5000000000000000, 870.0000000000000000, -20.00000000000001421 ) ) ;
#3934 = DIRECTION ( 'NONE',  ( 0.000000000000000000, 0.000000000000000000, 1.000000000000000000 ) ) ;
#3935 = PRODUCT_DEFINITION_SHAPE ( 'NONE', 'NONE',  #5392 ) ;
#3936 = ORIENTED_EDGE ( 'NONE', *, *, #4698, .F. ) ;
#3937 = CARTESIAN_POINT ( 'NONE',  ( 4.500000000000003553, -7.794228634059947147, 0.000000000000000000 ) ) ;
#3938 = DIRECTION ( 'NONE',  ( 0.000000000000000000, 0.000000000000000000, 1.000000000000000000 ) ) ;
#3939 = DIRECTION ( 'NONE',  ( -0.000000000000000000, -1.000000000000000000, -0.000000000000000000 ) ) ;
#3940 = DIRECTION ( 'NONE',  ( 1.000000000000000000, -0.000000000000000000, -0.000000000000000000 ) ) ;
#3941 = CARTESIAN_POINT ( 'NONE',  ( 6.000000000000000888, 0.000000000000000000, -25.03750572909317285 ) ) ;
#3942 = VERTEX_POINT ( 'NONE', #376 ) ;
#3943 = EDGE_CURVE ( 'NONE', #1224, #3280, #3314, .T. ) ;
#3944 = EDGE_CURVE ( 'NONE', #2006, #3569, #2521, .T. ) ;
#3945 = CARTESIAN_POINT ( 'NONE',  ( 9.473949623761187766, -1.924001493855441725, -9.141718809717339411 ) ) ;
#3946 = CARTESIAN_POINT ( 'NONE',  ( 0.7500000000000001110, 9.959292143521047080, -8.787392856021023491 ) ) ;
#3947 = ORIENTED_EDGE ( 'NONE', *, *, #2279, .F. ) ;
#3948 = APPLICATION_CONTEXT ( 'automotive_design' ) ;
#3949 = ORIENTED_EDGE ( 'NONE', *, *, #1592, .F. ) ;
#3950 = DIRECTION ( 'NONE',  ( 0.000000000000000000, 0.000000000000000000, 1.000000000000000000 ) ) ;
#3951 = ORIENTED_EDGE ( 'NONE', *, *, #4487, .T. ) ;
#3952 = CARTESIAN_POINT ( 'NONE',  ( 165.0000000000000000, 870.0000000000000000, 0.000000000000000000 ) ) ;
#3953 = DIRECTION ( 'NONE',  ( 1.000000000000000000, 0.000000000000000000, 0.000000000000000000 ) ) ;
#3954 = VECTOR ( 'NONE', #489, 1000.000000000000000 ) ;
#3955 = ORIENTED_EDGE ( 'NONE', *, *, #2721, .F. ) ;
#3956 = CARTESIAN_POINT ( 'NONE',  ( -1.603504855002233253E-16, 10.39230484541326582, -9.106320693283315393 ) ) ;
#3957 = PLANE ( 'NONE',  #4167 ) ;
#3958 = FACE_OUTER_BOUND ( 'NONE', #2837, .T. ) ;
#3959 = CARTESIAN_POINT ( 'NONE',  ( 9.370348127520008674, -5.409973013826442134, -9.628763110917944346 ) ) ;
#3960 = CIRCLE ( 'NONE', #636, 9.000000000000000000 ) ;
#3961 = PRODUCT_RELATED_PRODUCT_CATEGORY ( 'part', '', ( #2139 ) ) ;
#3962 = AXIS2_PLACEMENT_3D ( 'NONE', #1419, #1032, #289 ) ;
#3963 = CARTESIAN_POINT ( 'NONE',  ( -31.74999999999995737, 0.000000000000000000, 9.000000000000000000 ) ) ;
#3964 = CARTESIAN_POINT ( 'NONE',  ( 0.000000000000000000, 810.0000000000000000, 0.000000000000000000 ) ) ;
#3965 = CARTESIAN_POINT ( 'NONE',  ( 2.947989941763847543, 8.690282058967600420, -0.1432599722965993694 ) ) ;
#3966 = DIRECTION ( 'NONE',  ( 0.000000000000000000, 0.000000000000000000, 1.000000000000000000 ) ) ;
#3967 = LINE ( 'NONE', #254, #2429 ) ;
#3968 = AXIS2_PLACEMENT_3D ( 'NONE', #4803, #1112, #1080 ) ;
#3969 = ORIENTED_EDGE ( 'NONE', *, *, #1718, .F. ) ;
#3970 = SURFACE_STYLE_FILL_AREA ( #464 ) ;
#3971 = AXIS2_PLACEMENT_3D ( 'NONE', #4533, #789, #5362 ) ;
#3972 = EDGE_CURVE ( 'NONE', #838, #1279, #2883, .T. ) ;
#3973 = DIRECTION ( 'NONE',  ( 0.000000000000000000, 0.000000000000000000, 1.000000000000000000 ) ) ;
#3974 = DIRECTION ( 'NONE',  ( -0.000000000000000000, -0.000000000000000000, 1.000000000000000000 ) ) ;
#3975 = ORIENTED_EDGE ( 'NONE', *, *, #2913, .F. ) ;
#3976 =( NAMED_UNIT ( * ) PLANE_ANGLE_UNIT ( ) SI_UNIT ( $, .RADIAN. ) );
#3977 = ORIENTED_EDGE ( 'NONE', *, *, #1500, .T. ) ;
#3978 = AXIS2_PLACEMENT_3D ( 'NONE', #4470, #4910, #2471 ) ;
#3979 = AXIS2_PLACEMENT_3D ( 'NONE', #3086, #248, #2291 ) ;
#3980 = VERTEX_POINT ( 'NONE', #3796 ) ;
#3981 = DIRECTION ( 'NONE',  ( 1.000000000000000000, 0.000000000000000000, -0.000000000000000000 ) ) ;
#3982 = VECTOR ( 'NONE', #164, 1000.000000000000000 ) ;
#3983 = ORIENTED_EDGE ( 'NONE', *, *, #2847, .T. ) ;
#3984 = PLANE ( 'NONE',  #826 ) ;
#3985 = FACE_OUTER_BOUND ( 'NONE', #4365, .T. ) ;
#3986 = VECTOR ( 'NONE', #2094, 1000.000000000000000 ) ;
#3987 = ORIENTED_EDGE ( 'NONE', *, *, #2128, .F. ) ;
#3988 = ORIENTED_EDGE ( 'NONE', *, *, #470, .T. ) ;
#3989 = DIRECTION ( 'NONE',  ( 0.7071067811865577868, 8.659560562354808366E-17, 0.7071067811865373587 ) ) ;
#3990 = CARTESIAN_POINT ( 'NONE',  ( -7.780966735391496414, -5.899961606181325813, -9.200452032553489090 ) ) ;
#3991 = FACE_OUTER_BOUND ( 'NONE', #2835, .T. ) ;
#3992 = CARTESIAN_POINT ( 'NONE',  ( 0.000000000000000000, 810.0000000000000000, 0.000000000000000000 ) ) ;
#3993 = AXIS2_PLACEMENT_3D ( 'NONE', #2052, #3679, #749 ) ;
#3994 = EDGE_CURVE ( 'NONE', #3980, #3842, #2936, .T. ) ;
#3995 =( REPRESENTATION_RELATIONSHIP ('NONE','NONE', #4791, #3863 ) REPRESENTATION_RELATIONSHIP_WITH_TRANSFORMATION ( #919 )SHAPE_REPRESENTATION_RELATIONSHIP( ) );
#3996 = EDGE_LOOP ( 'NONE', ( #2786, #1456, #3815, #846 ) ) ;
#3997 = CIRCLE ( 'NONE', #3397, 6.499999999999983125 ) ;
#3998 = CIRCLE ( 'NONE', #4945, 6.499999999999988454 ) ;
#3999 = EDGE_CURVE ( 'NONE', #4039, #5330, #3362, .T. ) ;
#4000 = CARTESIAN_POINT ( 'NONE',  ( 9.000000000000001776, -5.196152422706638241, -1.199999999999999734 ) ) ;
#4001 = CARTESIAN_POINT ( 'NONE',  ( -6.329281523778169216, -7.289348427314507717, -9.189707035345833219 ) ) ;
#4002 = CARTESIAN_POINT ( 'NONE',  ( -1.566316456955016090, 10.05335742100714036, -9.380055053747698324 ) ) ;
#4003 = CYLINDRICAL_SURFACE ( 'NONE', #4323, 5.999999999999950262 ) ;
#4004 = CARTESIAN_POINT ( 'NONE',  ( -30.00000000000000355, 10.00000000000000000, -2.081668171172168908E-15 ) ) ;
#4005 = AXIS2_PLACEMENT_3D ( 'NONE', #3395, #2643, #3439 ) ;
#4006 = ORIENTED_EDGE ( 'NONE', *, *, #2481, .T. ) ;
#4007 = CONICAL_SURFACE ( 'NONE', #2339, 5.999999999999996447, 0.7853981633974074228 ) ;
#4008 = CARTESIAN_POINT ( 'NONE',  ( 9.498408982509888077, 4.628969134172655764, -9.525558946054186293 ) ) ;
#4009 = DIRECTION ( 'NONE',  ( 1.000000000000000000, 0.000000000000000000, 0.000000000000000000 ) ) ;
#4010 = ORIENTED_EDGE ( 'NONE', *, *, #4084, .T. ) ;
#4011 =( NAMED_UNIT ( * ) SI_UNIT ( $, .STERADIAN. ) SOLID_ANGLE_UNIT ( ) );
#4012 = EDGE_CURVE ( 'NONE', #3980, #4624, #2962, .T. ) ;
#4013 = ORIENTED_EDGE ( 'NONE', *, *, #3944, .T. ) ;
#4014 = CARTESIAN_POINT ( 'NONE',  ( 0.000000000000000000, 839.0360000000000582, -5.999999999999996447 ) ) ;
#4015 = EDGE_LOOP ( 'NONE', ( #5372, #1314, #1036, #4748 ) ) ;
#4016 = DIRECTION ( 'NONE',  ( 0.000000000000000000, -0.5000000000000008882, -0.8660254037844380415 ) ) ;
#4017 = CARTESIAN_POINT ( 'NONE',  ( -6.499999999999988454, 390.0000000000000000, -25.00000000000000000 ) ) ;
#4018 = ADVANCED_FACE ( 'NONE', ( #873, #2489 ), #1304, .F. ) ;
#4019 = EDGE_CURVE ( 'NONE', #2607, #428, #403, .T. ) ;
#4020 = ORIENTED_EDGE ( 'NONE', *, *, #3529, .F. ) ;
#4021 = CARTESIAN_POINT ( 'NONE',  ( 4.657533874636512748E-12, 10.81939018394125007, -9.628560800353234583 ) ) ;
#4022 = FACE_OUTER_BOUND ( 'NONE', #1377, .T. ) ;
#4023 = PLANE ( 'NONE',  #4582 ) ;
#4024 = CARTESIAN_POINT ( 'NONE',  ( -1.676835913137321903E-15, 35.00000000000000000, -25.00000000000000000 ) ) ;
#4025 = APPLICATION_PROTOCOL_DEFINITION ( 'draft international standard', 'automotive_design', 1998, #2167 ) ;
#4026 = VERTEX_POINT ( 'NONE', #4351 ) ;
#4027 = DIRECTION ( 'NONE',  ( 0.000000000000000000, 0.000000000000000000, 1.000000000000000000 ) ) ;
#4028 = VERTEX_POINT ( 'NONE', #257 ) ;
#4029 = CARTESIAN_POINT ( 'NONE',  ( -8.038218111920156501E-16, -10.97743472985186486, -9.686084310752816506 ) ) ;
#4030 = CARTESIAN_POINT ( 'NONE',  ( 121.7157287525372311, -20.00000000000000000, -136.7157287525388085 ) ) ;
#4031 = CARTESIAN_POINT ( 'NONE',  ( -1.144917494144692998E-14, 570.0000000000000000, -24.99999999999998579 ) ) ;
#4032 = CARTESIAN_POINT ( 'NONE',  ( -1.500000000000000666, -9.526279441628835443, -8.667800885990212478 ) ) ;
#4033 = CARTESIAN_POINT ( 'NONE',  ( 9.000000000000000000, 1.887153537675259285, -8.512871225629151439 ) ) ;
#4034 = DIRECTION ( 'NONE',  ( -1.000000000000000000, 0.000000000000000000, 0.000000000000000000 ) ) ;
#4035 = ORIENTED_EDGE ( 'NONE', *, *, #5360, .F. ) ;
#4036 =( NAMED_UNIT ( * ) PLANE_ANGLE_UNIT ( ) SI_UNIT ( $, .RADIAN. ) );
#4037 = ORIENTED_EDGE ( 'NONE', *, *, #310, .F. ) ;
#4038 = EDGE_CURVE ( 'NONE', #2114, #3040, #1624, .T. ) ;
#4039 = VERTEX_POINT ( 'NONE', #2745 ) ;
#4040 = FILL_AREA_STYLE ('',( #590 ) ) ;
#4041 = ORIENTED_EDGE ( 'NONE', *, *, #4019, .F. ) ;
#4042 = FACE_OUTER_BOUND ( 'NONE', #4518, .T. ) ;
#4043 = FILL_AREA_STYLE_COLOUR ( '', #1700 ) ;
#4044 = ORIENTED_EDGE ( 'NONE', *, *, #3542, .F. ) ;
#4045 = CARTESIAN_POINT ( 'NONE',  ( -6.430436718082018110, 6.679690475221754298, -0.2264046624879764436 ) ) ;
#4046 = CARTESIAN_POINT ( 'NONE',  ( -0.3968280142502572660, -10.16319608456390355, -8.848996304169316929 ) ) ;
#4047 = FACE_OUTER_BOUND ( 'NONE', #1584, .T. ) ;
#4048 = FACE_OUTER_BOUND ( 'NONE', #2949, .T. ) ;
#4049 = DIRECTION ( 'NONE',  ( 1.000000000000000000, 0.000000000000000000, 0.000000000000000000 ) ) ;
#4050 = ADVANCED_FACE ( 'NONE', ( #1105 ), #4772, .F. ) ;
#4051 = AXIS2_PLACEMENT_3D ( 'NONE', #620, #4844, #3136 ) ;
#4052 = ORIENTED_EDGE ( 'NONE', *, *, #4181, .T. ) ;
#4053 = ORIENTED_EDGE ( 'NONE', *, *, #4953, .F. ) ;
#4054 = CARTESIAN_POINT ( 'NONE',  ( -6.499999999999988454, 390.0000000000000000, 25.00000000000000000 ) ) ;
#4055 = AXIS2_PLACEMENT_3D ( 'NONE', #3361, #1351, #4301 ) ;
#4056 = ORIENTED_EDGE ( 'NONE', *, *, #4401, .F. ) ;
#4057 = FILL_AREA_STYLE_COLOUR ( '', #4773 ) ;
#4058 = CARTESIAN_POINT ( 'NONE',  ( -9.506737344437272696, 5.488717364925923548, -9.686084310752812954 ) ) ;
#4059 = FACE_BOUND ( 'NONE', #2086, .T. ) ;
#4060 = CYLINDRICAL_SURFACE ( 'NONE', #4666, 5.999999999999950262 ) ;
#4061 = VECTOR ( 'NONE', #4364, 1000.000000000000000 ) ;
#4062 = DIRECTION ( 'NONE',  ( -0.000000000000000000, 1.000000000000000000, -0.000000000000000000 ) ) ;
#4063 = CARTESIAN_POINT ( 'NONE',  ( 7.347880794884115792E-16, 839.0360000000000582, 5.999999999999996447 ) ) ;
#4064 = AXIS2_PLACEMENT_3D ( 'NONE', #889, #2914, #4547 ) ;
#4065 = EDGE_LOOP ( 'NONE', ( #1077, #5133, #645, #4711 ) ) ;
#4066 = CIRCLE ( 'NONE', #3798, 5.099999999999999645 ) ;
#4067 = AXIS2_PLACEMENT_3D ( 'NONE', #1115, #263, #4488 ) ;
#4068 = DIRECTION ( 'NONE',  ( -0.000000000000000000, 0.000000000000000000, 1.000000000000000000 ) ) ;
#4069 = CARTESIAN_POINT ( 'NONE',  ( 12.59999999999999964, 0.000000000000000000, 6.000000000000001776 ) ) ;
#4070 = EDGE_LOOP ( 'NONE', ( #3320, #1751, #2933, #3691 ) ) ;
#4071 = DIRECTION ( 'NONE',  ( -1.387778780781445676E-16, 0.000000000000000000, -1.000000000000000000 ) ) ;
#4072 = DIRECTION ( 'NONE',  ( 0.000000000000000000, -0.000000000000000000, 1.000000000000000000 ) ) ;
#4073 = CIRCLE ( 'NONE', #5369, 5.099999999999999645 ) ;
#4074 = B_SPLINE_CURVE_WITH_KNOTS ( 'NONE', 3,
 ( #3937, #546, #1046, #3482, #1382, #655 ),
 .UNSPECIFIED., .F., .F.,
 ( 4, 2, 4 ),
 ( 0.005333245961717292087, 0.007986067645924077585, 0.01063888933013086222 ),
 .UNSPECIFIED. ) ;
#4075 = VECTOR ( 'NONE', #1129, 1000.000000000000000 ) ;
#4076 = AXIS2_PLACEMENT_3D ( 'NONE', #3677, #695, #2356 ) ;
#4077 = VERTEX_POINT ( 'NONE', #1051 ) ;
#4078 = DIRECTION ( 'NONE',  ( -1.000000000000000000, -0.000000000000000000, 0.000000000000000000 ) ) ;
#4079 = FACE_OUTER_BOUND ( 'NONE', #1162, .T. ) ;
#4080 = CARTESIAN_POINT ( 'NONE',  ( -139.9999999999999716, 870.0000000000000000, -5.999999999999950262 ) ) ;
#4081 = UNCERTAINTY_MEASURE_WITH_UNIT (LENGTH_MEASURE( 1.000000000000000082E-05 ), #4993, 'distance_accuracy_value', 'NONE');
#4082 = SHAPE_DEFINITION_REPRESENTATION ( #493, #3275 ) ;
#4083 = AXIS2_PLACEMENT_3D ( 'NONE', #880, #2155, #856 ) ;
#4084 = EDGE_CURVE ( 'NONE', #4077, #1160, #4644, .T. ) ;
#4085 = DIRECTION ( 'NONE',  ( 1.000000000000000000, 0.000000000000000000, 0.000000000000000000 ) ) ;
#4086 = VERTEX_POINT ( 'NONE', #3151 ) ;
#4087 = CARTESIAN_POINT ( 'NONE',  ( 0.000000000000000000, 0.000000000000000000, 0.000000000000000000 ) ) ;
#4088 = FACE_OUTER_BOUND ( 'NONE', #3682, .T. ) ;
#4089 = CARTESIAN_POINT ( 'NONE',  ( 9.506737344437272696, 5.488717364925924436, -9.686084310752812954 ) ) ;
#4090 = AXIS2_PLACEMENT_3D ( 'NONE', #2533, #4662, #835 ) ;
#4091 = EDGE_LOOP ( 'NONE', ( #693, #3784, #3868, #396 ) ) ;
#4092 = DIRECTION ( 'NONE',  ( -0.000000000000000000, -0.000000000000000000, 1.000000000000000000 ) ) ;
#4093 = PRODUCT_DEFINITION_CONTEXT ( 'detailed design', #3109, 'design' ) ;
#4094 = LINE ( 'NONE', #5363, #2688 ) ;
#4095 = VECTOR ( 'NONE', #4814, 1000.000000000000000 ) ;
#4096 = ORIENTED_EDGE ( 'NONE', *, *, #794, .T. ) ;
#4097 =( NAMED_UNIT ( * ) PLANE_ANGLE_UNIT ( ) SI_UNIT ( $, .RADIAN. ) );
#4098 = LINE ( 'NONE', #1504, #999 ) ;
#4099 = DIRECTION ( 'NONE',  ( 1.000000000000000000, 0.000000000000000000, 0.000000000000000000 ) ) ;
#4100 = ADVANCED_FACE ( 'NONE', ( #85 ), #231, .T. ) ;
#4101 = ORIENTED_EDGE ( 'NONE', *, *, #5050, .T. ) ;
#4102 =( LENGTH_UNIT ( ) NAMED_UNIT ( * ) SI_UNIT ( .MILLI., .METRE. ) );
#4103 = EDGE_CURVE ( 'NONE', #2036, #4833, #1323, .T. ) ;
#4104 = ORIENTED_EDGE ( 'NONE', *, *, #1301, .F. ) ;
#4105 = CARTESIAN_POINT ( 'NONE',  ( 137.5000000000000000, 870.0000000000000000, 0.000000000000000000 ) ) ;
#4106 = DIRECTION ( 'NONE',  ( -0.000000000000000000, -0.000000000000000000, 1.000000000000000000 ) ) ;
#4107 = CARTESIAN_POINT ( 'NONE',  ( 0.000000000000000000, 570.0000000000000000, -25.00000000000000000 ) ) ;
#4108 = DIRECTION ( 'NONE',  ( 1.000000000000000000, 0.000000000000000000, 0.000000000000000000 ) ) ;
#4109 = EDGE_CURVE ( 'NONE', #3267, #2355, #5068, .T. ) ;
#4110 = CARTESIAN_POINT ( 'NONE',  ( -9.000000000000000000, -5.196152422706636465, -12.00000000000000000 ) ) ;
#4111 = DIRECTION ( 'NONE',  ( -1.000000000000000000, -0.000000000000000000, -0.000000000000000000 ) ) ;
#4112 = SURFACE_SIDE_STYLE ('',( #362 ) ) ;
#4113 = CARTESIAN_POINT ( 'NONE',  ( 0.000000000000000000, 390.0000000000000000, 25.00000000000000000 ) ) ;
#4114 = FACE_OUTER_BOUND ( 'NONE', #2993, .T. ) ;
#4115 = CARTESIAN_POINT ( 'NONE',  ( 25.00000000000000000, 610.0000000000000000, -25.00000000000000000 ) ) ;
#4116 = CARTESIAN_POINT ( 'NONE',  ( -2.999999999999999112, 8.660254037844383745, -8.505011083697292307 ) ) ;
#4117 = EDGE_LOOP ( 'NONE', ( #3500, #409, #2878, #2109 ) ) ;
#4118 = EDGE_CURVE ( 'NONE', #5233, #4122, #1445, .T. ) ;
#4119 = EDGE_LOOP ( 'NONE', ( #705, #4272, #351, #5336 ) ) ;
#4120 = EDGE_CURVE ( 'NONE', #3600, #2478, #1413, .T. ) ;
#4121 = DIRECTION ( 'NONE',  ( -0.000000000000000000, 1.000000000000000000, -0.000000000000000000 ) ) ;
#4122 = VERTEX_POINT ( 'NONE', #5252 ) ;
#4123 = SURFACE_SIDE_STYLE ('',( #2141 ) ) ;
#4124 = ORIENTED_EDGE ( 'NONE', *, *, #3814, .T. ) ;
#4125 = EDGE_LOOP ( 'NONE', ( #160, #238 ) ) ;
#4126 = FACE_OUTER_BOUND ( 'NONE', #5128, .T. ) ;
#4127 = CARTESIAN_POINT ( 'NONE',  ( -6.331831610933253529, 7.287864996261684603, -9.189462574975657105 ) ) ;
#4128 = DIRECTION ( 'NONE',  ( 1.000000000000000000, 0.000000000000000000, 0.000000000000000000 ) ) ;
#4129 = CARTESIAN_POINT ( 'NONE',  ( 3.070858717647242386, -9.166611990350897798, -9.141698485139787778 ) ) ;
#4130 = APPLICATION_PROTOCOL_DEFINITION ( 'draft international standard', 'automotive_design', 1998, #2458 ) ;
#4131 = LINE ( 'NONE', #1149, #390 ) ;
#4132 = FACE_OUTER_BOUND ( 'NONE', #120, .T. ) ;
#4133 = PRODUCT_DEFINITION ( 'UNKNOWN', '', #840, #2824 ) ;
#4134 = PLANE ( 'NONE',  #1101 ) ;
#4135 = DIRECTION ( 'NONE',  ( 0.000000000000000000, -1.000000000000000000, 1.188187522481193495E-15 ) ) ;
#4136 = AXIS2_PLACEMENT_3D ( 'NONE', #2856, #4501, #34 ) ;
#4137 = ORIENTED_EDGE ( 'NONE', *, *, #1066, .F. ) ;
#4138 = CARTESIAN_POINT ( 'NONE',  ( -6.499999999999984901, 35.00000000000000000, 30.00000000000000711 ) ) ;
#4139 = CARTESIAN_POINT ( 'NONE',  ( 6.499999999999981348, 35.00000000000000000, -25.00000000000000000 ) ) ;
#4140 = ORIENTED_EDGE ( 'NONE', *, *, #533, .T. ) ;
#4141 = CIRCLE ( 'NONE', #5167, 5.036000000000040444 ) ;
#4142 = ORIENTED_EDGE ( 'NONE', *, *, #3506, .T. ) ;
#4143 = ADVANCED_FACE ( 'NONE', ( #4256 ), #1499, .T. ) ;
#4144 = VECTOR ( 'NONE', #1179, 1000.000000000000000 ) ;
#4145 = DIRECTION ( 'NONE',  ( 1.000000000000000000, 0.000000000000000000, 2.081668171172168513E-16 ) ) ;
#4146 = ORIENTED_EDGE ( 'NONE', *, *, #1898, .F. ) ;
#4147 = VERTEX_POINT ( 'NONE', #1074 ) ;
#4148 = AXIS2_PLACEMENT_3D ( 'NONE', #4665, #2194, #4295 ) ;
#4149 = ORIENTED_EDGE ( 'NONE', *, *, #2467, .T. ) ;
#4150 = EDGE_LOOP ( 'NONE', ( #2010, #1319 ) ) ;
#4151 = VECTOR ( 'NONE', #505, 1000.000000000000000 ) ;
#4152 = DIRECTION ( 'NONE',  ( -0.000000000000000000, -0.000000000000000000, -1.000000000000000000 ) ) ;
#4153 = DIRECTION ( 'NONE',  ( 1.000000000000000000, 0.000000000000000000, 0.000000000000000000 ) ) ;
#4154 = AXIS2_PLACEMENT_3D ( 'NONE', #2434, #5290, #769 ) ;
#4155 = DIRECTION ( 'NONE',  ( 0.000000000000000000, -0.000000000000000000, 1.000000000000000000 ) ) ;
#4156 = CARTESIAN_POINT ( 'NONE',  ( 1.499235438989850788, -10.09238013695879133, -9.361164777499757506 ) ) ;
#4157 = CONTEXT_DEPENDENT_SHAPE_REPRESENTATION ( #1023, #576 ) ;
#4158 = AXIS2_PLACEMENT_3D ( 'NONE', #1217, #2050, #5356 ) ;
#4159 = ORIENTED_EDGE ( 'NONE', *, *, #3943, .T. ) ;
#4160 = LINE ( 'NONE', #3371, #3554 ) ;
#4161 = DIRECTION ( 'NONE',  ( -1.000000000000000000, -0.000000000000000000, -0.000000000000000000 ) ) ;
#4162 = CARTESIAN_POINT ( 'NONE',  ( 0.6000000000000033085, 0.000000000000000000, 0.000000000000000000 ) ) ;
#4163 = EDGE_CURVE ( 'NONE', #1969, #1397, #3174, .T. ) ;
#4164 = CARTESIAN_POINT ( 'NONE',  ( 3.000000000000000000, -8.660254037844392627, -8.505011083697295859 ) ) ;
#4165 = VECTOR ( 'NONE', #3122, 1000.000000000000000 ) ;
#4166 = EDGE_CURVE ( 'NONE', #2065, #4039, #586, .T. ) ;
#4167 = AXIS2_PLACEMENT_3D ( 'NONE', #210, #5100, #3081 ) ;
#4168 = ORIENTED_EDGE ( 'NONE', *, *, #380, .T. ) ;
#4169 = CARTESIAN_POINT ( 'NONE',  ( -2.352990130084610634E-16, 10.39230484541326582, -12.00000000000000000 ) ) ;
#4170 = CARTESIAN_POINT ( 'NONE',  ( 6.000000000000000000, 6.193651186687738874E-16, -5.057500000000000107 ) ) ;
#4171 = ORIENTED_EDGE ( 'NONE', *, *, #5313, .F. ) ;
#4172 = CIRCLE ( 'NONE', #2068, 6.000000000000000000 ) ;
#4173 = ORIENTED_EDGE ( 'NONE', *, *, #4627, .F. ) ;
#4174 = CARTESIAN_POINT ( 'NONE',  ( -6.000000000000005329, 570.0000000000000000, -24.03599999999999071 ) ) ;
#4175 = ORIENTED_EDGE ( 'NONE', *, *, #2969, .T. ) ;
#4176 = ADVANCED_BREP_SHAPE_REPRESENTATION ( '', ( #1819, #4154 ), #2853 ) ;
#4177 = ORIENTED_EDGE ( 'NONE', *, *, #1959, .F. ) ;
#4178 = DIRECTION ( 'NONE',  ( -1.000000000000000000, -0.000000000000000000, -0.000000000000000000 ) ) ;
#4179 = LINE ( 'NONE', #5018, #3986 ) ;
#4180 = CARTESIAN_POINT ( 'NONE',  ( -9.000000000000000000, -3.516072269208510903, -0.5641419778896283876 ) ) ;
#4181 = EDGE_CURVE ( 'NONE', #2978, #4754, #1854, .T. ) ;
#4182 = ADVANCED_FACE ( 'NONE', ( #634 ), #4426, .F. ) ;
#4183 = DIRECTION ( 'NONE',  ( 0.000000000000000000, -1.000000000000000000, 0.000000000000000000 ) ) ;
#4184 = DIRECTION ( 'NONE',  ( 0.000000000000000000, 0.000000000000000000, -1.000000000000000000 ) ) ;
#4185 = CARTESIAN_POINT ( 'NONE',  ( 0.000000000000000000, -2.919948986426526893, 5.057500000000001883 ) ) ;
#4186 = CARTESIAN_POINT ( 'NONE',  ( 1.500000000000000000, -9.526279441628833666, -8.667800885990210702 ) ) ;
#4187 = ORIENTED_EDGE ( 'NONE', *, *, #4084, .F. ) ;
#4188 = ORIENTED_EDGE ( 'NONE', *, *, #4218, .F. ) ;
#4189 =( NAMED_UNIT ( * ) PLANE_ANGLE_UNIT ( ) SI_UNIT ( $, .RADIAN. ) );
#4190 = UNCERTAINTY_MEASURE_WITH_UNIT (LENGTH_MEASURE( 1.000000000000000082E-05 ), #3858, 'distance_accuracy_value', 'NONE');
#4191 = FACE_BOUND ( 'NONE', #1478, .T. ) ;
#4192 = EDGE_LOOP ( 'NONE', ( #4956, #1058, #1111, #3351 ) ) ;
#4193 = EDGE_LOOP ( 'NONE', ( #3056, #5176 ) ) ;
#4194 = CARTESIAN_POINT ( 'NONE',  ( 0.000000000000000000, 2.919948986426526005, -5.057500000000002771 ) ) ;
#4195 = ORIENTED_EDGE ( 'NONE', *, *, #992, .T. ) ;
#4196 = EDGE_CURVE ( 'NONE', #5142, #1861, #4848, .T. ) ;
#4197 = ORIENTED_EDGE ( 'NONE', *, *, #1491, .T. ) ;
#4198 = CARTESIAN_POINT ( 'NONE',  ( -121.7157287525381122, -20.00000000000000000, 121.7157287525380127 ) ) ;
#4199 = DIRECTION ( 'NONE',  ( -0.000000000000000000, -0.000000000000000000, 1.000000000000000000 ) ) ;
#4200 = FACE_OUTER_BOUND ( 'NONE', #2024, .T. ) ;
#4201 = EDGE_CURVE ( 'NONE', #4754, #3771, #4591, .T. ) ;
#4202 = FACE_OUTER_BOUND ( 'NONE', #3443, .T. ) ;
#4203 = LINE ( 'NONE', #2986, #2229 ) ;
#4204 = CARTESIAN_POINT ( 'NONE',  ( -0.7181044661681214025, -9.977707038564833653, -0.8426663529491328353 ) ) ;
#4205 = CARTESIAN_POINT ( 'NONE',  ( 0.000000000000000000, -10.39230484541327293, -8.935996291721338025 ) ) ;
#4206 = ADVANCED_FACE ( 'NONE', ( #1647 ), #317, .F. ) ;
#4207 = DIRECTION ( 'NONE',  ( -0.000000000000000000, -0.000000000000000000, -1.000000000000000000 ) ) ;
#4208 = SURFACE_SIDE_STYLE ('',( #1693 ) ) ;
#4209 = VERTEX_POINT ( 'NONE', #3327 ) ;
#4210 = EDGE_LOOP ( 'NONE', ( #153, #2513 ) ) ;
#4211 = DIRECTION ( 'NONE',  ( -0.000000000000000000, 1.000000000000000000, -0.000000000000000000 ) ) ;
#4212 = CARTESIAN_POINT ( 'NONE',  ( 9.000000000000001776, 0.000000000000000000, 0.000000000000000000 ) ) ;
#4213 = B_SPLINE_CURVE_WITH_KNOTS ( 'NONE', 3,
 ( #4212, #426, #2085, #447, #2105, #4632, #3786, #1754, #4612, #885, #478, #905 ),
 .UNSPECIFIED., .F., .F.,
 ( 4, 2, 2, 2, 2, 4 ),
 ( 0.01261372891313921468, 0.01327902839800527111, 0.01394432788287132928, 0.01527492685260344214, 0.01660552582233555674, 0.01793612479206766960 ),
 .UNSPECIFIED. ) ;
#4214 = ORIENTED_EDGE ( 'NONE', *, *, #3841, .T. ) ;
#4215 = VECTOR ( 'NONE', #2013, 999.9999999999998863 ) ;
#4216 = FACE_OUTER_BOUND ( 'NONE', #44, .T. ) ;
#4217 = VECTOR ( 'NONE', #1479, 1000.000000000000000 ) ;
#4218 = EDGE_CURVE ( 'NONE', #966, #1510, #4094, .T. ) ;
#4219 = SURFACE_SIDE_STYLE ('',( #5011 ) ) ;
#4220 = ORIENTED_EDGE ( 'NONE', *, *, #908, .T. ) ;
#4221 = MECHANICAL_DESIGN_GEOMETRIC_PRESENTATION_REPRESENTATION (  '', ( #4912 ), #1855 ) ;
#4222 = ORIENTED_EDGE ( 'NONE', *, *, #688, .T. ) ;
#4223 = CARTESIAN_POINT ( 'NONE',  ( 6.000000000000000000, -2.919948986426526893, 5.057500000000001883 ) ) ;
#4224 = DIRECTION ( 'NONE',  ( -0.000000000000000000, -1.000000000000000000, -0.000000000000000000 ) ) ;
#4225 = CARTESIAN_POINT ( 'NONE',  ( 8.249999999999998224, 5.629165124598849879, -8.787392856021023491 ) ) ;
#4226 = PLANE ( 'NONE',  #3662 ) ;
#4227 = CIRCLE ( 'NONE', #1858, 6.000000000000000000 ) ;
#4228 = PRODUCT_DEFINITION_FORMATION_WITH_SPECIFIED_SOURCE ( 'ANY', '', #3432, .NOT_KNOWN. ) ;
#4229 = ORIENTED_EDGE ( 'NONE', *, *, #817, .T. ) ;
#4230 = AXIS2_PLACEMENT_3D ( 'NONE', #756, #1582, #904 ) ;
#4231 = CARTESIAN_POINT ( 'NONE',  ( -8.999999999999998224, 0.4512186429437706758, -0.007346088320835175017 ) ) ;
#4232 = DIRECTION ( 'NONE',  ( -0.000000000000000000, -0.000000000000000000, 1.000000000000000000 ) ) ;
#4233 = DIRECTION ( 'NONE',  ( 1.000000000000000000, 0.000000000000000000, 0.000000000000000000 ) ) ;
#4234 = DIRECTION ( 'NONE',  ( -6.938893903907228378E-17, 0.000000000000000000, 1.000000000000000000 ) ) ;
#4235 = PRESENTATION_STYLE_ASSIGNMENT (( #2185 ) ) ;
#4236 = VECTOR ( 'NONE', #3504, 999.9999999999998863 ) ;
#4237 = EDGE_CURVE ( 'NONE', #3600, #4283, #5280, .T. ) ;
#4238 = MECHANICAL_DESIGN_GEOMETRIC_PRESENTATION_REPRESENTATION (  '', ( #2138 ), #916 ) ;
#4239 = VERTEX_POINT ( 'NONE', #4063 ) ;
#4240 = AXIS2_PLACEMENT_3D ( 'NONE', #3879, #3476, #2732 ) ;
#4241 = ORIENTED_EDGE ( 'NONE', *, *, #609, .F. ) ;
#4242 =( NAMED_UNIT ( * ) PLANE_ANGLE_UNIT ( ) SI_UNIT ( $, .RADIAN. ) );
#4243 = MECHANICAL_DESIGN_GEOMETRIC_PRESENTATION_REPRESENTATION (  '', ( #5023 ), #1876 ) ;
#4244 = CARTESIAN_POINT ( 'NONE',  ( 92.00000000000000000, 6.757601037695095565E-16, -5.035999999999999588 ) ) ;
#4245 = DIRECTION ( 'NONE',  ( 1.000000000000000000, 0.000000000000000000, 0.000000000000000000 ) ) ;
#4246 = VERTEX_POINT ( 'NONE', #4534 ) ;
#4247 = EDGE_CURVE ( 'NONE', #503, #3744, #1192, .T. ) ;
#4248 = AXIS2_PLACEMENT_3D ( 'NONE', #355, #2440, #269 ) ;
#4249 = DIRECTION ( 'NONE',  ( 1.000000000000000000, 0.000000000000000000, 0.000000000000000000 ) ) ;
#4250 = SURFACE_STYLE_USAGE ( .BOTH. , #2699 ) ;
#4251 = AXIS2_PLACEMENT_3D ( 'NONE', #2319, #299, #1903 ) ;
#4252 = ADVANCED_FACE ( 'NONE', ( #5339 ), #4948, .F. ) ;
#4253 = ORIENTED_EDGE ( 'NONE', *, *, #1905, .F. ) ;
#4254 = CARTESIAN_POINT ( 'NONE',  ( 0.000000000000000000, 810.0000000000000000, -5.999999999999998224 ) ) ;
#4255 = DIRECTION ( 'NONE',  ( 0.000000000000000000, 0.000000000000000000, 1.000000000000000000 ) ) ;
#4256 = FACE_OUTER_BOUND ( 'NONE', #188, .T. ) ;
#4257 = CYLINDRICAL_SURFACE ( 'NONE', #780, 6.499999999999988454 ) ;
#4258 = VECTOR ( 'NONE', #1422, 1000.000000000000000 ) ;
#4259 = CONTEXT_DEPENDENT_SHAPE_REPRESENTATION ( #943, #3548 ) ;
#4260 = CARTESIAN_POINT ( 'NONE',  ( -9.000000000000001776, 4.367518130255689357, -0.8586158810094310923 ) ) ;
#4261 = VERTEX_POINT ( 'NONE', #4139 ) ;
#4262 = CYLINDRICAL_SURFACE ( 'NONE', #2762, 6.499999999999988454 ) ;
#4263 = DIRECTION ( 'NONE',  ( -1.000000000000000000, -0.000000000000000000, -0.000000000000000000 ) ) ;
#4264 = FACE_BOUND ( 'NONE', #5216, .T. ) ;
#4265 = CARTESIAN_POINT ( 'NONE',  ( 0.7500000000000001110, -9.959292143521054186, -8.787392856021027043 ) ) ;
#4266 = ADVANCED_FACE ( 'NONE', ( #2361 ), #2426, .T. ) ;
#4267 = CARTESIAN_POINT ( 'NONE',  ( 7.990639863760086392, 6.344566044897808510, -9.361164777499386247 ) ) ;
#4268 = DIRECTION ( 'NONE',  ( -0.000000000000000000, -0.000000000000000000, 1.000000000000000000 ) ) ;
#4269 = DIRECTION ( 'NONE',  ( 0.000000000000000000, 0.4999999999999990008, -0.8660254037844392627 ) ) ;
#4270 = ADVANCED_FACE ( 'NONE', ( #4890 ), #5114, .T. ) ;
#4271 = EDGE_CURVE ( 'NONE', #2509, #2607, #893, .T. ) ;
#4272 = ORIENTED_EDGE ( 'NONE', *, *, #4395, .F. ) ;
#4273 = AXIS2_PLACEMENT_3D ( 'NONE', #580, #3885, #143 ) ;
#4274 = DIRECTION ( 'NONE',  ( 1.000000000000000000, 0.000000000000000000, 0.000000000000000000 ) ) ;
#4275 = CARTESIAN_POINT ( 'NONE',  ( 0.000000000000000000, 510.0000000000000000, 25.00000000000000000 ) ) ;
#4276 = PRODUCT_DEFINITION_SHAPE ( 'NONE', 'NONE',  #5398 ) ;
#4277 = MECHANICAL_DESIGN_GEOMETRIC_PRESENTATION_REPRESENTATION (  '', ( #1750 ), #1665 ) ;
#4278 = DIRECTION ( 'NONE',  ( -1.000000000000000000, 0.000000000000000000, -0.000000000000000000 ) ) ;
#4279 = VERTEX_POINT ( 'NONE', #5312 ) ;
#4280 = LINE ( 'NONE', #3058, #2162 ) ;
#4281 = CARTESIAN_POINT ( 'NONE',  ( 25.00000000000000000, 10.00000000000000000, 25.00000000000000711 ) ) ;
#4282 = CARTESIAN_POINT ( 'NONE',  ( -121.7157287525392917, 0.000000000000000000, -121.7157287525368332 ) ) ;
#4283 = VERTEX_POINT ( 'NONE', #1559 ) ;
#4284 = DIRECTION ( 'NONE',  ( 0.000000000000000000, 0.000000000000000000, 1.000000000000000000 ) ) ;
#4285 = CARTESIAN_POINT ( 'NONE',  ( 0.000000000000000000, 0.000000000000000000, 0.000000000000000000 ) ) ;
#4286 = ADVANCED_BREP_SHAPE_REPRESENTATION ( '', ( #104, #4154 ), #3189 ) ;
#4287 = DIRECTION ( 'NONE',  ( 0.000000000000000000, -0.000000000000000000, 1.000000000000000000 ) ) ;
#4288 = ORIENTED_EDGE ( 'NONE', *, *, #1481, .F. ) ;
#4289 = DIRECTION ( 'NONE',  ( 0.000000000000000000, 0.000000000000000000, -1.000000000000000000 ) ) ;
#4290 = DIRECTION ( 'NONE',  ( 8.659560562354580336E-17, -0.7071067811865765496, 0.7071067811865185959 ) ) ;
#4291 = LINE ( 'NONE', #4631, #4151 ) ;
#4292 = PRODUCT_DEFINITION_CONTEXT ( 'detailed design', #1156, 'design' ) ;
#4293 = CARTESIAN_POINT ( 'NONE',  ( 6.000000000000000000, -4.379923479639802331, -2.528749999999995612 ) ) ;
#4294 = PRODUCT_DEFINITION_SHAPE ( 'NONE', 'NONE',  #2536 ) ;
#4295 = DIRECTION ( 'NONE',  ( 0.000000000000000000, 0.000000000000000000, -1.000000000000000000 ) ) ;
#4296 =( LENGTH_UNIT ( ) NAMED_UNIT ( * ) SI_UNIT ( .MILLI., .METRE. ) );
#4297 = EDGE_CURVE ( 'NONE', #5294, #4433, #2830, .T. ) ;
#4298 = CIRCLE ( 'NONE', #1769, 6.499999999999983125 ) ;
#4299 = ORIENTED_EDGE ( 'NONE', *, *, #992, .F. ) ;
#4300 = DIRECTION ( 'NONE',  ( -0.000000000000000000, -0.000000000000000000, 1.000000000000000000 ) ) ;
#4301 = DIRECTION ( 'NONE',  ( -1.000000000000000000, 0.000000000000000000, 0.000000000000000000 ) ) ;
#4302 = CARTESIAN_POINT ( 'NONE',  ( -24.99999999999999645, 610.0000000000000000, -25.00000000000000000 ) ) ;
#4303 = CIRCLE ( 'NONE', #40, 15.00000000000000000 ) ;
#4304 = EDGE_LOOP ( 'NONE', ( #2424, #4352 ) ) ;
#4305 = VECTOR ( 'NONE', #746, 1000.000000000000000 ) ;
#4306 = ORIENTED_EDGE ( 'NONE', *, *, #3927, .F. ) ;
#4307 = DIRECTION ( 'NONE',  ( 1.000000000000000000, -0.000000000000000000, -0.000000000000000000 ) ) ;
#4308 = CARTESIAN_POINT ( 'NONE',  ( 25.00000000000000000, 810.0000000000000000, -25.00000000000000000 ) ) ;
#4309 = DIRECTION ( 'NONE',  ( 0.000000000000000000, 0.000000000000000000, 1.000000000000000000 ) ) ;
#4310 = CARTESIAN_POINT ( 'NONE',  ( 9.506737344437272696, -5.488717364925930653, -9.686084310752812954 ) ) ;
#4311 = CARTESIAN_POINT ( 'NONE',  ( 0.000000000000000000, 0.000000000000000000, 0.000000000000000000 ) ) ;
#4312 = CIRCLE ( 'NONE', #644, 5.057500000000000107 ) ;
#4313 = PRESENTATION_LAYER_ASSIGNMENT (  '', '', ( #4730 ) ) ;
#4314 = ADVANCED_FACE ( 'NONE', ( #4915 ), #725, .F. ) ;
#4315 = CARTESIAN_POINT ( 'NONE',  ( 30.00000000000000355, 610.0000000000000000, -30.00000000000000355 ) ) ;
#4316 = CARTESIAN_POINT ( 'NONE',  ( 139.9999999999999716, 810.0000000000000000, -25.00000000000000000 ) ) ;
#4317 = DIRECTION ( 'NONE',  ( -0.000000000000000000, 1.000000000000000000, 0.000000000000000000 ) ) ;
#4318 = PRODUCT_DEFINITION_FORMATION_WITH_SPECIFIED_SOURCE ( 'ANY', '', #443, .NOT_KNOWN. ) ;
#4319 = DIRECTION ( 'NONE',  ( 0.000000000000000000, 0.000000000000000000, -1.000000000000000000 ) ) ;
#4320 = DIRECTION ( 'NONE',  ( -0.000000000000000000, -0.000000000000000000, 1.000000000000000000 ) ) ;
#4321 = AXIS2_PLACEMENT_3D ( 'NONE', #4348, #192, #3966 ) ;
#4322 = EDGE_CURVE ( 'NONE', #428, #5213, #2866, .T. ) ;
#4323 = AXIS2_PLACEMENT_3D ( 'NONE', #1495, #2772, #4823 ) ;
#4324 = FACE_OUTER_BOUND ( 'NONE', #2927, .T. ) ;
#4325 =( LENGTH_UNIT ( ) NAMED_UNIT ( * ) SI_UNIT ( .MILLI., .METRE. ) );
#4326 = AXIS2_PLACEMENT_3D ( 'NONE', #5332, #784, #2893 ) ;
#4327 = EDGE_CURVE ( 'NONE', #1418, #1702, #4172, .T. ) ;
#4328 = VECTOR ( 'NONE', #4399, 1000.000000000000000 ) ;
#4329 = ORIENTED_EDGE ( 'NONE', *, *, #1029, .F. ) ;
#4330 = FACE_OUTER_BOUND ( 'NONE', #3268, .T. ) ;
#4331 = DIRECTION ( 'NONE',  ( -1.000000000000000000, -0.000000000000000000, -0.000000000000000000 ) ) ;
#4332 = CARTESIAN_POINT ( 'NONE',  ( 137.5000000000000000, 870.0000000000000000, 0.000000000000000000 ) ) ;
#4333 = CIRCLE ( 'NONE', #4503, 5.099999999999999645 ) ;
#4334 = ORIENTED_EDGE ( 'NONE', *, *, #2160, .T. ) ;
#4335 = VERTEX_POINT ( 'NONE', #1368 ) ;
#4336 = CARTESIAN_POINT ( 'NONE',  ( -1.144917494144692998E-14, 570.0000000000000000, 30.00000000000001066 ) ) ;
#4337 = DIRECTION ( 'NONE',  ( -0.000000000000000000, 1.000000000000000000, -0.000000000000000000 ) ) ;
#4338 = AXIS2_PLACEMENT_3D ( 'NONE', #5298, #4902, #776 ) ;
#4339 = DIRECTION ( 'NONE',  ( -1.000000000000000000, -0.000000000000000000, -0.000000000000000000 ) ) ;
#4340 = ORIENTED_EDGE ( 'NONE', *, *, #937, .T. ) ;
#4341 = EDGE_CURVE ( 'NONE', #1489, #5294, #5059, .T. ) ;
#4342 = DIRECTION ( 'NONE',  ( 0.000000000000000000, 0.000000000000000000, -1.000000000000000000 ) ) ;
#4343 = ADVANCED_FACE ( 'NONE', ( #4191, #3864 ), #1697, .T. ) ;
#4344 = VERTEX_POINT ( 'NONE', #1338 ) ;
#4345 = PLANE ( 'NONE',  #1688 ) ;
#4346 = DIRECTION ( 'NONE',  ( -0.000000000000000000, 1.000000000000000000, 0.000000000000000000 ) ) ;
#4347 = PLANE ( 'NONE',  #3105 ) ;
#4348 = CARTESIAN_POINT ( 'NONE',  ( 0.000000000000000000, 820.0000000000001137, 0.000000000000000000 ) ) ;
#4349 = CARTESIAN_POINT ( 'NONE',  ( 25.00000000000000000, 610.0000000000000000, 25.00000000000000711 ) ) ;
#4350 = CARTESIAN_POINT ( 'NONE',  ( 9.000000000000000000, 5.678793296733535279, -9.021743630911338130 ) ) ;
#4351 = CARTESIAN_POINT ( 'NONE',  ( -25.00000000000000000, 10.00000000000000000, 24.99999999999999645 ) ) ;
#4352 = ORIENTED_EDGE ( 'NONE', *, *, #3286, .T. ) ;
#4353 = VERTEX_POINT ( 'NONE', #2997 ) ;
#4354 = ORIENTED_EDGE ( 'NONE', *, *, #2312, .T. ) ;
#4355 = DIRECTION ( 'NONE',  ( -6.938893903907228378E-17, 0.000000000000000000, 1.000000000000000000 ) ) ;
#4356 = CARTESIAN_POINT ( 'NONE',  ( -6.499999999999988454, 510.0000000000000000, 25.00000000000000000 ) ) ;
#4357 = ORIENTED_EDGE ( 'NONE', *, *, #2338, .T. ) ;
#4358 = CARTESIAN_POINT ( 'NONE',  ( -4.894105558640187148, 7.566691683689904302, 2.037114238146591921E-15 ) ) ;
#4359 = SURFACE_STYLE_USAGE ( .BOTH. , #1039 ) ;
#4360 = CARTESIAN_POINT ( 'NONE',  ( 25.00000000000000000, 10.00000000000000000, 25.00000000000000711 ) ) ;
#4361 = CARTESIAN_POINT ( 'NONE',  ( 139.9999999999999716, 810.0000000000000000, 25.00000000000000000 ) ) ;
#4362 = ADVANCED_FACE ( 'NONE', ( #1776 ), #3350, .F. ) ;
#4363 = VERTEX_POINT ( 'NONE', #2166 ) ;
#4364 = DIRECTION ( 'NONE',  ( -1.000000000000000000, -0.000000000000000000, -0.000000000000000000 ) ) ;
#4365 = EDGE_LOOP ( 'NONE', ( #4453, #1086, #1464, #3911 ) ) ;
#4366 = CARTESIAN_POINT ( 'NONE',  ( -7.923304691439486014, -6.383148552592252223, -9.380055053747694771 ) ) ;
#4367 = CARTESIAN_POINT ( 'NONE',  ( 91.03600000000004400, 0.000000000000000000, 6.000000000000000888 ) ) ;
#4368 = CARTESIAN_POINT ( 'NONE',  ( -6.245004513516506329E-15, 557.4999999999997726, 30.00000000000000711 ) ) ;
#4369 = CARTESIAN_POINT ( 'NONE',  ( -137.5000000000000000, 870.0000000000000000, 20.00000000000001421 ) ) ;
#4370 = CARTESIAN_POINT ( 'NONE',  ( 9.489875848528154023, -3.747870292144412474, -9.361175357011155995 ) ) ;
#4371 = DIRECTION ( 'NONE',  ( -1.000000000000000000, 0.000000000000000000, 0.000000000000000000 ) ) ;
#4372 = ORIENTED_EDGE ( 'NONE', *, *, #3481, .T. ) ;
#4373 = ORIENTED_EDGE ( 'NONE', *, *, #2876, .F. ) ;
#4374 = PLANE ( 'NONE',  #3626 ) ;
#4375 = EDGE_CURVE ( 'NONE', #5361, #932, #4786, .T. ) ;
#4376 = EDGE_LOOP ( 'NONE', ( #5088, #795, #3184 ) ) ;
#4377 = CARTESIAN_POINT ( 'NONE',  ( 7.960204194457795477E-16, 820.0000000000001137, -6.500000000000000000 ) ) ;
#4378 = CYLINDRICAL_SURFACE ( 'NONE', #4067, 5.099999999999999645 ) ;
#4379 = ADVANCED_FACE ( 'NONE', ( #1673, #935 ), #3836, .T. ) ;
#4380 = AXIS2_PLACEMENT_3D ( 'NONE', #4723, #243, #1484 ) ;
#4381 = ORIENTED_EDGE ( 'NONE', *, *, #2613, .T. ) ;
#4382 = ORIENTED_EDGE ( 'NONE', *, *, #5006, .T. ) ;
#4383 = DIRECTION ( 'NONE',  ( 0.000000000000000000, 0.000000000000000000, 1.000000000000000000 ) ) ;
#4384 = CARTESIAN_POINT ( 'NONE',  ( -9.333481574700599026, -5.003616745783467046, -9.543752552345290852 ) ) ;
#4385 = CARTESIAN_POINT ( 'NONE',  ( -9.000000000000000000, 4.330127018922190096, -8.787392856021023491 ) ) ;
#4386 = DIRECTION ( 'NONE',  ( 0.000000000000000000, -0.000000000000000000, 1.000000000000000000 ) ) ;
#4387 = AXIS2_PLACEMENT_3D ( 'NONE', #5145, #1894, #3133 ) ;
#4388 = VERTEX_POINT ( 'NONE', #1731 ) ;
#4389 = ORIENTED_EDGE ( 'NONE', *, *, #3994, .F. ) ;
#4390 = DIRECTION ( 'NONE',  ( -0.000000000000000000, -0.000000000000000000, 1.000000000000000000 ) ) ;
#4391 = DIRECTION ( 'NONE',  ( 0.000000000000000000, 0.000000000000000000, 1.000000000000000000 ) ) ;
#4392 = FACE_OUTER_BOUND ( 'NONE', #3348, .T. ) ;
#4393 = LINE ( 'NONE', #659, #761 ) ;
#4394 = DIRECTION ( 'NONE',  ( 0.000000000000000000, 0.000000000000000000, -1.000000000000000000 ) ) ;
#4395 = EDGE_CURVE ( 'NONE', #3851, #3942, #2133, .T. ) ;
#4396 = AXIS2_PLACEMENT_3D ( 'NONE', #1246, #4456, #3665 ) ;
#4397 = AXIS2_PLACEMENT_3D ( 'NONE', #4685, #2971, #3016 ) ;
#4398 = LINE ( 'NONE', #3918, #3534 ) ;
#4399 = DIRECTION ( 'NONE',  ( -6.938893903907228378E-17, 0.000000000000000000, 1.000000000000000000 ) ) ;
#4400 = VERTEX_POINT ( 'NONE', #4588 ) ;
#4401 = EDGE_CURVE ( 'NONE', #4261, #2639, #4415, .T. ) ;
#4402 = ADVANCED_FACE ( 'NONE', ( #866 ), #2972, .T. ) ;
#4403 = VECTOR ( 'NONE', #3123, 1000.000000000000227 ) ;
#4404 = PRESENTATION_LAYER_ASSIGNMENT (  '', '', ( #2669 ) ) ;
#4405 = ORIENTED_EDGE ( 'NONE', *, *, #3999, .F. ) ;
#4406 = FACE_OUTER_BOUND ( 'NONE', #4817, .T. ) ;
#4407 = ORIENTED_EDGE ( 'NONE', *, *, #1827, .F. ) ;
#4408 = DIRECTION ( 'NONE',  ( 1.000000000000000000, 0.000000000000000000, 0.000000000000000000 ) ) ;
#4409 = EDGE_CURVE ( 'NONE', #601, #2534, #4213, .T. ) ;
#4410 = ORIENTED_EDGE ( 'NONE', *, *, #1253, .F. ) ;
#4411 = CARTESIAN_POINT ( 'NONE',  ( 25.00000000000000000, 610.0000000000000000, 25.00000000000000711 ) ) ;
#4412 = CARTESIAN_POINT ( 'NONE',  ( 4.500000000000003553, 7.794228634059947147, 0.000000000000000000 ) ) ;
#4413 = FACE_OUTER_BOUND ( 'NONE', #3577, .T. ) ;
#4414 = DIRECTION ( 'NONE',  ( 0.000000000000000000, 0.000000000000000000, 1.000000000000000000 ) ) ;
#4415 = CIRCLE ( 'NONE', #502, 6.499999999999983125 ) ;
#4416 = SHAPE_DEFINITION_REPRESENTATION ( #1810, #2934 ) ;
#4417 = CARTESIAN_POINT ( 'NONE',  ( -31.74999999999995737, 7.347880794884121708E-16, -6.000000000000001776 ) ) ;
#4418 = ORIENTED_EDGE ( 'NONE', *, *, #3999, .T. ) ;
#4419 = DIRECTION ( 'NONE',  ( 0.000000000000000000, 1.000000000000000000, -0.000000000000000000 ) ) ;
#4420 = CARTESIAN_POINT ( 'NONE',  ( -12.38940648156203750, 1.517264699098042146E-15, -10.20000000000000107 ) ) ;
#4421 = EDGE_CURVE ( 'NONE', #3771, #4754, #4333, .T. ) ;
#4422 = DIRECTION ( 'NONE',  ( -1.000000000000000000, -0.000000000000000000, -0.000000000000000000 ) ) ;
#4423 = LINE ( 'NONE', #389, #3557 ) ;
#4424 = ORIENTED_EDGE ( 'NONE', *, *, #16, .F. ) ;
#4425 = DIRECTION ( 'NONE',  ( -1.000000000000000000, -0.000000000000000000, -0.000000000000000000 ) ) ;
#4426 = CYLINDRICAL_SURFACE ( 'NONE', #2870, 6.499999999999983125 ) ;
#4427 = ORIENTED_EDGE ( 'NONE', *, *, #3542, .T. ) ;
#4428 = VERTEX_POINT ( 'NONE', #1850 ) ;
#4429 = EDGE_CURVE ( 'NONE', #745, #5042, #4797, .T. ) ;
#4430 = DIRECTION ( 'NONE',  ( -0.000000000000000000, -0.000000000000000000, 1.000000000000000000 ) ) ;
#4431 = DIRECTION ( 'NONE',  ( -0.000000000000000000, -0.000000000000000000, 1.000000000000000000 ) ) ;
#4432 = EDGE_CURVE ( 'NONE', #1397, #966, #3092, .T. ) ;
#4433 = VERTEX_POINT ( 'NONE', #605 ) ;
#4434 = DIRECTION ( 'NONE',  ( -0.8660254037844383745, -0.5000000000000003331, 0.000000000000000000 ) ) ;
#4435 = CIRCLE ( 'NONE', #1131, 9.000000000000001776 ) ;
#4436 = FACE_OUTER_BOUND ( 'NONE', #3742, .T. ) ;
#4437 = ORIENTED_EDGE ( 'NONE', *, *, #4608, .F. ) ;
#4438 = DIRECTION ( 'NONE',  ( 1.000000000000000000, 0.000000000000000000, 0.000000000000000000 ) ) ;
#4439 = CARTESIAN_POINT ( 'NONE',  ( 7.546085493343360540, 6.035570354503541068, -0.5405968996908940838 ) ) ;
#4440 = CYLINDRICAL_SURFACE ( 'NONE', #4840, 6.499999999999988454 ) ;
#4441 = DIRECTION ( 'NONE',  ( -0.000000000000000000, -1.000000000000000000, -0.000000000000000000 ) ) ;
#4442 = UNCERTAINTY_MEASURE_WITH_UNIT (LENGTH_MEASURE( 1.000000000000000082E-05 ), #1465, 'distance_accuracy_value', 'NONE');
#4443 = APPLICATION_PROTOCOL_DEFINITION ( 'draft international standard', 'automotive_design', 1998, #3948 ) ;
#4444 = ORIENTED_EDGE ( 'NONE', *, *, #3576, .F. ) ;
#4445 = DIRECTION ( 'NONE',  ( -0.000000000000000000, -0.000000000000000000, 1.000000000000000000 ) ) ;
#4446 = CARTESIAN_POINT ( 'NONE',  ( -137.5000000000000000, 870.0000000000000000, -6.000000000000006217 ) ) ;
#4447 = CARTESIAN_POINT ( 'NONE',  ( 5.999999999999983125, 570.0000000000000000, -24.03599999999999071 ) ) ;
#4448 = FACE_OUTER_BOUND ( 'NONE', #486, .T. ) ;
#4449 = ORIENTED_EDGE ( 'NONE', *, *, #2743, .F. ) ;
#4450 = PRODUCT_DEFINITION_SHAPE ( 'NONE', 'NONE',  #5395 ) ;
#4451 = CARTESIAN_POINT ( 'NONE',  ( 9.244715922125774199, 5.337439226220936028, -9.530716183751501092 ) ) ;
#4452 = CARTESIAN_POINT ( 'NONE',  ( 6.000000000000000000, 2.919948986426526005, -5.057500000000002771 ) ) ;
#4453 = ORIENTED_EDGE ( 'NONE', *, *, #5241, .T. ) ;
#4454 = VERTEX_POINT ( 'NONE', #1049 ) ;
#4455 = ORIENTED_EDGE ( 'NONE', *, *, #115, .F. ) ;
#4456 = DIRECTION ( 'NONE',  ( -0.000000000000000000, -0.000000000000000000, 1.000000000000000000 ) ) ;
#4457 = VERTEX_POINT ( 'NONE', #630 ) ;
#4458 = SURFACE_STYLE_USAGE ( .BOTH. , #3222 ) ;
#4459 = ADVANCED_FACE ( 'NONE', ( #193 ), #4746, .F. ) ;
#4460 = ORIENTED_EDGE ( 'NONE', *, *, #2896, .T. ) ;
#4461 = CARTESIAN_POINT ( 'NONE',  ( 6.499999999999988454, 510.0000000000000000, -25.00000000000000000 ) ) ;
#4462 = CARTESIAN_POINT ( 'NONE',  ( 0.000000000000000000, 0.000000000000000000, 0.000000000000000000 ) ) ;
#4463 = DIRECTION ( 'NONE',  ( 0.000000000000000000, 0.000000000000000000, 1.000000000000000000 ) ) ;
#4464 = CARTESIAN_POINT ( 'NONE',  ( 150.0000000000000000, 870.0000000000000000, 0.000000000000000000 ) ) ;
#4465 = PRODUCT_CONTEXT ( 'NONE', #788, 'mechanical' ) ;
#4466 = AXIS2_PLACEMENT_3D ( 'NONE', #2405, #7, #2882 ) ;
#4467 = DIRECTION ( 'NONE',  ( 1.000000000000000000, 0.000000000000000000, 0.000000000000000000 ) ) ;
#4468 = DIRECTION ( 'NONE',  ( -0.000000000000000000, 1.000000000000000000, -0.000000000000000000 ) ) ;
#4469 = PRESENTATION_STYLE_ASSIGNMENT (( #308 ) ) ;
#4470 = CARTESIAN_POINT ( 'NONE',  ( 92.00000000000000000, 0.000000000000000000, 0.000000000000000000 ) ) ;
#4471 = CARTESIAN_POINT ( 'NONE',  ( -9.058806161333684770, -5.230104175782646969, -9.269265075619308902 ) ) ;
#4472 = AXIS2_PLACEMENT_3D ( 'NONE', #3822, #124, #513 ) ;
#4473 = EDGE_CURVE ( 'NONE', #2478, #3488, #3967, .T. ) ;
#4474 = ORIENTED_EDGE ( 'NONE', *, *, #4566, .T. ) ;
#4475 = DIRECTION ( 'NONE',  ( 0.000000000000000000, 0.000000000000000000, -1.000000000000000000 ) ) ;
#4476 = DIRECTION ( 'NONE',  ( 0.000000000000000000, -1.000000000000000000, 1.039664082171044284E-15 ) ) ;
#4477 = ADVANCED_FACE ( 'NONE', ( #2633 ), #551, .T. ) ;
#4478 = ORIENTED_EDGE ( 'NONE', *, *, #862, .T. ) ;
#4479 = ORIENTED_EDGE ( 'NONE', *, *, #52, .F. ) ;
#4480 = VERTEX_POINT ( 'NONE', #4293 ) ;
#4481 = ORIENTED_EDGE ( 'NONE', *, *, #5118, .F. ) ;
#4482 = ORIENTED_EDGE ( 'NONE', *, *, #4540, .T. ) ;
#4483 = VECTOR ( 'NONE', #3457, 1000.000000000000000 ) ;
#4484 = DIRECTION ( 'NONE',  ( -1.000000000000000000, 0.000000000000000000, -0.000000000000000000 ) ) ;
#4485 = CARTESIAN_POINT ( 'NONE',  ( 0.000000000000000000, 820.0000000000001137, 0.000000000000000000 ) ) ;
#4486 = VERTEX_POINT ( 'NONE', #1910 ) ;
#4487 = EDGE_CURVE ( 'NONE', #5257, #5200, #2659, .T. ) ;
#4488 = DIRECTION ( 'NONE',  ( 1.000000000000000000, 0.000000000000000000, 0.000000000000000000 ) ) ;
#4489 = VECTOR ( 'NONE', #1329, 1000.000000000000000 ) ;
#4490 = AXIS2_PLACEMENT_3D ( 'NONE', #1598, #5237, #2850 ) ;
#4491 = VECTOR ( 'NONE', #2857, 1000.000000000000000 ) ;
#4492 = ORIENTED_EDGE ( 'NONE', *, *, #2792, .T. ) ;
#4493 = DIRECTION ( 'NONE',  ( 0.000000000000000000, 0.000000000000000000, 1.000000000000000000 ) ) ;
#4494 = LINE ( 'NONE', #4785, #1361 ) ;
#4495 = PLANE ( 'NONE',  #3647 ) ;
#4496 = LINE ( 'NONE', #5326, #3475 ) ;
#4497 = CONTEXT_DEPENDENT_SHAPE_REPRESENTATION ( #1993, #1012 ) ;
#4498 = COLOUR_RGB ( '',0.8941176470588234615, 0.8941176470588234615, 0.8941176470588234615 ) ;
#4499 = ADVANCED_FACE ( 'NONE', ( #3531 ), #1885, .T. ) ;
#4500 = DIRECTION ( 'NONE',  ( -0.000000000000000000, -0.000000000000000000, -1.000000000000000000 ) ) ;
#4501 = DIRECTION ( 'NONE',  ( -0.000000000000000000, -0.000000000000000000, -1.000000000000000000 ) ) ;
#4502 = CARTESIAN_POINT ( 'NONE',  ( -25.00000000000000000, 10.00000000000000000, -25.00000000000000000 ) ) ;
#4503 = AXIS2_PLACEMENT_3D ( 'NONE', #506, #3429, #5082 ) ;
#4504 = DIRECTION ( 'NONE',  ( 1.000000000000000000, 0.000000000000000000, 0.000000000000000000 ) ) ;
#4505 = ADVANCED_FACE ( 'NONE', ( #1020 ), #1802, .T. ) ;
#4506 = CARTESIAN_POINT ( 'NONE',  ( -7.500000000000000000, -6.062177826491077504, -8.667800885990208926 ) ) ;
#4507 = VERTEX_POINT ( 'NONE', #583 ) ;
#4508 = AXIS2_PLACEMENT_3D ( 'NONE', #3448, #3499, #975 ) ;
#4509 = PLANE ( 'NONE',  #3971 ) ;
#4510 = CARTESIAN_POINT ( 'NONE',  ( -2.352990130084610634E-16, 10.39230484541326582, -8.935996291721336249 ) ) ;
#4511 = VECTOR ( 'NONE', #4625, 1000.000000000000000 ) ;
#4512 = VERTEX_POINT ( 'NONE', #1468 ) ;
#4513 = VECTOR ( 'NONE', #1308, 1000.000000000000000 ) ;
#4514 = EDGE_LOOP ( 'NONE', ( #982, #1859, #322 ) ) ;
#4515 = LINE ( 'NONE', #2455, #906 ) ;
#4516 = ORIENTED_EDGE ( 'NONE', *, *, #3814, .F. ) ;
#4517 = PRODUCT_DEFINITION ( 'UNKNOWN', '', #2053, #4093 ) ;
#4518 = EDGE_LOOP ( 'NONE', ( #5056, #202, #4427, #3648, #4886 ) ) ;
#4519 = DIRECTION ( 'NONE',  ( 1.000000000000000000, 0.000000000000000000, 0.000000000000000000 ) ) ;
#4520 = CARTESIAN_POINT ( 'NONE',  ( -1.171714802207773687, 9.715814988945137287, -8.684787165852368318 ) ) ;
#4521 = FACE_BOUND ( 'NONE', #2362, .T. ) ;
#4522 = CARTESIAN_POINT ( 'NONE',  ( 3.049442433610978414E-16, 10.97743472985185775, -9.686084310752812954 ) ) ;
#4523 = SHAPE_DEFINITION_REPRESENTATION ( #2589, #121 ) ;
#4524 = CARTESIAN_POINT ( 'NONE',  ( 6.000000000000000000, 0.000000000000000000, 0.000000000000000000 ) ) ;
#4525 = EDGE_LOOP ( 'NONE', ( #1657, #2588 ) ) ;
#4526 = FACE_OUTER_BOUND ( 'NONE', #2729, .T. ) ;
#4527 = CARTESIAN_POINT ( 'NONE',  ( -25.00000000000000000, 210.0000000000000284, 24.99999999999999645 ) ) ;
#4528 = CARTESIAN_POINT ( 'NONE',  ( 25.00000000000000000, 810.0000000000000000, 25.00000000000000711 ) ) ;
#4529 = EDGE_CURVE ( 'NONE', #1888, #2898, #1884, .T. ) ;
#4530 = PRODUCT ( 'Locking handle', 'Locking handle', '', ( #2765 ) ) ;
#4531 = VECTOR ( 'NONE', #1907, 1000.000000000000114 ) ;
#4532 = VERTEX_POINT ( 'NONE', #147 ) ;
#4533 = CARTESIAN_POINT ( 'NONE',  ( 0.000000000000000000, -10.39230484541327293, -12.00000000000000000 ) ) ;
#4534 = CARTESIAN_POINT ( 'NONE',  ( 6.000000000000000000, 2.919948986426538440, 5.057499999999994778 ) ) ;
#4535 = VERTEX_POINT ( 'NONE', #4369 ) ;
#4536 = ORIENTED_EDGE ( 'NONE', *, *, #4473, .T. ) ;
#4537 = DIRECTION ( 'NONE',  ( -0.000000000000000000, -0.000000000000000000, 1.000000000000000000 ) ) ;
#4538 = EDGE_LOOP ( 'NONE', ( #1656, #4372, #4146, #2029 ) ) ;
#4539 = ORIENTED_EDGE ( 'NONE', *, *, #156, .T. ) ;
#4540 = EDGE_CURVE ( 'NONE', #2438, #3240, #1536, .T. ) ;
#4541 = ORIENTED_EDGE ( 'NONE', *, *, #3667, .F. ) ;
#4542 = DIRECTION ( 'NONE',  ( -1.000000000000000000, -0.000000000000000000, -0.000000000000000000 ) ) ;
#4543 = DIRECTION ( 'NONE',  ( -0.000000000000000000, -0.000000000000000000, -1.000000000000000000 ) ) ;
#4544 = CARTESIAN_POINT ( 'NONE',  ( -1.676835913137321903E-15, 35.00000000000000000, 25.00000000000000000 ) ) ;
#4545 = CARTESIAN_POINT ( 'NONE',  ( 1.219033264610904554, -9.688495661941223247, -9.200452032562273175 ) ) ;
#4546 = ADVANCED_FACE ( 'NONE', ( #1070 ), #2241, .T. ) ;
#4547 = DIRECTION ( 'NONE',  ( 0.000000000000000000, 0.000000000000000000, -1.000000000000000000 ) ) ;
#4548 = ORIENTED_EDGE ( 'NONE', *, *, #2983, .F. ) ;
#4549 = CARTESIAN_POINT ( 'NONE',  ( -1.388245801416654908E-12, -10.81994602764950386, -9.628763110917946122 ) ) ;
#4550 = PLANE ( 'NONE',  #1619 ) ;
#4551 = FACE_OUTER_BOUND ( 'NONE', #3787, .T. ) ;
#4552 = LINE ( 'NONE', #3424, #3820 ) ;
#4553 = VERTEX_POINT ( 'NONE', #2246 ) ;
#4554 = CIRCLE ( 'NONE', #381, 15.00000000000000000 ) ;
#4555 = VERTEX_POINT ( 'NONE', #3563 ) ;
#4556 = VECTOR ( 'NONE', #896, 999.9999999999998863 ) ;
#4557 = LINE ( 'NONE', #4138, #652 ) ;
#4558 = CARTESIAN_POINT ( 'NONE',  ( -121.7157287525392917, -20.00000000000000000, -121.7157287525368332 ) ) ;
#4559 = ORIENTED_EDGE ( 'NONE', *, *, #5238, .T. ) ;
#4560 = TOROIDAL_SURFACE ( 'NONE', #480, 12.07201791628681598, 0.9279820837131842470 ) ;
#4561 = VERTEX_POINT ( 'NONE', #3486 ) ;
#4562 = VECTOR ( 'NONE', #3120, 1000.000000000000000 ) ;
#4563 = DIRECTION ( 'NONE',  ( 1.000000000000000000, 0.000000000000000000, 0.000000000000000000 ) ) ;
#4564 = EDGE_CURVE ( 'NONE', #4951, #2404, #1831, .T. ) ;
#4565 = ORIENTED_EDGE ( 'NONE', *, *, #2473, .T. ) ;
#4566 = EDGE_CURVE ( 'NONE', #3517, #2863, #4708, .T. ) ;
#4567 = CLOSED_SHELL ( 'NONE', ( #5138, #4459, #5342, #3690, #1455, #1928, #5374, #1272, #618, #3617, #2370, #1617, #3163, #1315, #1889, #2926, #3098, #3827, #4505, #2502, #1014, #264, #1874, #3830, #5115, #4739, #2253, #3923, #2516, #1363, #2695, #3119 ) ) ;
#4568 = AXIS2_PLACEMENT_3D ( 'NONE', #2209, #1488, #1064 ) ;
#4569 = ORIENTED_EDGE ( 'NONE', *, *, #517, .F. ) ;
#4570 = VECTOR ( 'NONE', #4660, 1000.000000000000000 ) ;
#4571 = VERTEX_POINT ( 'NONE', #5161 ) ;
#4572 = CARTESIAN_POINT ( 'NONE',  ( 6.499999999999988454, 450.0000000000000000, 25.00000000000000000 ) ) ;
#4573 = CARTESIAN_POINT ( 'NONE',  ( 6.499999999999988454, 510.0000000000000000, 25.00000000000000000 ) ) ;
#4574 = CARTESIAN_POINT ( 'NONE',  ( 0.000000000000000000, 820.0000000000001137, 0.000000000000000000 ) ) ;
#4575 = AXIS2_PLACEMENT_3D ( 'NONE', #858, #64, #2918 ) ;
#4576 = COLOUR_RGB ( '',0.8941176470588234615, 0.8941176470588234615, 0.8941176470588234615 ) ;
#4577 = CIRCLE ( 'NONE', #3197, 6.000000000000005329 ) ;
#4578 = DIRECTION ( 'NONE',  ( 1.000000000000000000, 0.000000000000000000, 0.000000000000000000 ) ) ;
#4579 =( NAMED_UNIT ( * ) SI_UNIT ( $, .STERADIAN. ) SOLID_ANGLE_UNIT ( ) );
#4580 = CARTESIAN_POINT ( 'NONE',  ( -0.7169666604817549471, 9.978363950984137531, -0.8432325327665461945 ) ) ;
#4581 = CARTESIAN_POINT ( 'NONE',  ( -9.477393160736850675, -1.839800711185081150, -9.189479368578805207 ) ) ;
#4582 = AXIS2_PLACEMENT_3D ( 'NONE', #4901, #799, #2039 ) ;
#4583 = AXIS2_PLACEMENT_3D ( 'NONE', #1025, #196, #2332 ) ;
#4584 = ADVANCED_FACE ( 'NONE', ( #1410 ), #4737, .T. ) ;
#4585 = ORIENTED_EDGE ( 'NONE', *, *, #365, .F. ) ;
#4586 = CARTESIAN_POINT ( 'NONE',  ( 0.000000000000000000, 0.000000000000000000, 0.000000000000000000 ) ) ;
#4587 = LINE ( 'NONE', #42, #4483 ) ;
#4588 = CARTESIAN_POINT ( 'NONE',  ( 4.500000000000003553, -7.794228634059947147, 0.000000000000000000 ) ) ;
#4589 = ORIENTED_EDGE ( 'NONE', *, *, #1387, .F. ) ;
#4590 = ORIENTED_EDGE ( 'NONE', *, *, #2621, .T. ) ;
#4591 = CIRCLE ( 'NONE', #1022, 5.099999999999999645 ) ;
#4592 = ORIENTED_EDGE ( 'NONE', *, *, #4931, .T. ) ;
#4593 = AXIS2_PLACEMENT_3D ( 'NONE', #37, #926, #2608 ) ;
#4594 = DIRECTION ( 'NONE',  ( 0.000000000000000000, 0.4999999999999991118, -0.8660254037844391517 ) ) ;
#4595 = VERTEX_POINT ( 'NONE', #3294 ) ;
#4596 =( NAMED_UNIT ( * ) SI_UNIT ( $, .STERADIAN. ) SOLID_ANGLE_UNIT ( ) );
#4597 = EDGE_CURVE ( 'NONE', #3517, #752, #931, .T. ) ;
#4598 = ORIENTED_EDGE ( 'NONE', *, *, #3708, .F. ) ;
#4599 = DIRECTION ( 'NONE',  ( 1.000000000000000000, 0.000000000000000000, 0.000000000000000000 ) ) ;
#4600 = DIRECTION ( 'NONE',  ( -0.000000000000000000, -0.000000000000000000, -1.000000000000000000 ) ) ;
#4601 = CARTESIAN_POINT ( 'NONE',  ( -4.500000000000002665, -7.794228634059946259, 0.000000000000000000 ) ) ;
#4602 = DIRECTION ( 'NONE',  ( -0.8191520442889915765, 1.003171929053524500E-16, 0.5735764363510464925 ) ) ;
#4603 = EDGE_LOOP ( 'NONE', ( #2908, #4229, #4171, #792 ) ) ;
#4604 = CARTESIAN_POINT ( 'NONE',  ( 121.7157287525384533, -20.00000000000000000, 136.7157287525376717 ) ) ;
#4605 = PRESENTATION_STYLE_ASSIGNMENT (( #419 ) ) ;
#4606 = DIRECTION ( 'NONE',  ( 0.000000000000000000, -0.000000000000000000, -1.000000000000000000 ) ) ;
#4607 = CARTESIAN_POINT ( 'NONE',  ( 25.00000000000000000, 610.0000000000000000, -25.00000000000000000 ) ) ;
#4608 = EDGE_CURVE ( 'NONE', #4959, #5234, #4923, .T. ) ;
#4609 = ORIENTED_EDGE ( 'NONE', *, *, #5238, .F. ) ;
#4610 = LINE ( 'NONE', #729, #965 ) ;
#4611 = PLANE ( 'NONE',  #1781 ) ;
#4612 = CARTESIAN_POINT ( 'NONE',  ( 8.999999999999998224, 3.519160108721334002, -0.5651793076691169482 ) ) ;
#4613 = ORIENTED_EDGE ( 'NONE', *, *, #2776, .F. ) ;
#4614 = PRODUCT_DEFINITION_SHAPE ( 'NONE', 'NONE',  #255 ) ;
#4615 = DIRECTION ( 'NONE',  ( -0.000000000000000000, -0.000000000000000000, 1.000000000000000000 ) ) ;
#4616 = ORIENTED_EDGE ( 'NONE', *, *, #3430, .T. ) ;
#4617 = ORIENTED_EDGE ( 'NONE', *, *, #179, .T. ) ;
#4618 = CARTESIAN_POINT ( 'NONE',  ( -25.00000000000000000, 810.0000000000000000, 24.99999999999999645 ) ) ;
#4619 = ADVANCED_FACE ( 'NONE', ( #4448 ), #4060, .F. ) ;
#4620 = CARTESIAN_POINT ( 'NONE',  ( -150.0000000000000000, 810.0000000000000000, 25.00000000000000000 ) ) ;
#4621 = CARTESIAN_POINT ( 'NONE',  ( -8.283033339518246052, -5.610093317135764757, -0.8432325327665481929 ) ) ;
#4622 = FACE_BOUND ( 'NONE', #4985, .T. ) ;
#4623 = VERTEX_POINT ( 'NONE', #786 ) ;
#4624 = VERTEX_POINT ( 'NONE', #4943 ) ;
#4625 = DIRECTION ( 'NONE',  ( 0.000000000000000000, 1.000000000000000000, 0.000000000000000000 ) ) ;
#4626 = LINE ( 'NONE', #5076, #1610 ) ;
#4627 = EDGE_CURVE ( 'NONE', #2006, #1452, #2895, .T. ) ;
#4628 = CARTESIAN_POINT ( 'NONE',  ( -9.000000000000000000, -1.887523386541274828, -8.512900682043403222 ) ) ;
#4629 = ORIENTED_EDGE ( 'NONE', *, *, #708, .F. ) ;
#4630 = SURFACE_STYLE_FILL_AREA ( #5080 ) ;
#4631 = CARTESIAN_POINT ( 'NONE',  ( 6.499999999999981348, 35.00000000000000000, 30.00000000000000711 ) ) ;
#4632 = CARTESIAN_POINT ( 'NONE',  ( 9.000000000000001776, 1.787897550172802275, -0.1425508600568101969 ) ) ;
#4633 = EDGE_CURVE ( 'NONE', #4965, #3420, #1390, .T. ) ;
#4634 = AXIS2_PLACEMENT_3D ( 'NONE', #1087, #1118, #3930 ) ;
#4635 = ADVANCED_FACE ( 'NONE', ( #4114 ), #3705, .F. ) ;
#4636 = CYLINDRICAL_SURFACE ( 'NONE', #909, 5.999999999999996447 ) ;
#4637 = CIRCLE ( 'NONE', #2300, 6.600000000000001421 ) ;
#4638 = SHAPE_REPRESENTATION_RELATIONSHIP ( 'NONE' , 'NONE' ,  #1620, #5266 ) ;
#4639=STYLED_ITEM('',(#5433),#1819);
#4640 = ORIENTED_EDGE ( 'NONE', *, *, #4564, .T. ) ;
#4641 = ADVANCED_FACE ( 'NONE', ( #1957 ), #1608, .F. ) ;
#4642 = LINE ( 'NONE', #1758, #1414 ) ;
#4643 = DIRECTION ( 'NONE',  ( 1.000000000000000000, 0.000000000000000000, 0.000000000000000000 ) ) ;
#4644 = LINE ( 'NONE', #3508, #4328 ) ;
#4645 = CARTESIAN_POINT ( 'NONE',  ( -9.000000000000000000, -5.196152422706636465, -1.199999999999999734 ) ) ;
#4646 = AXIS2_PLACEMENT_3D ( 'NONE', #2089, #350, #323 ) ;
#4647 = AXIS2_PLACEMENT_3D ( 'NONE', #316, #4062, #2389 ) ;
#4648 = COLOUR_RGB ( '',0.8941176470588234615, 0.8941176470588234615, 0.8941176470588234615 ) ;
#4649 = DIRECTION ( 'NONE',  ( 0.000000000000000000, 0.000000000000000000, -1.000000000000000000 ) ) ;
#4650 = CARTESIAN_POINT ( 'NONE',  ( 9.473745496805527466, -0.9176529770164938427, -9.138786188337402194 ) ) ;
#4651 = PRESENTATION_STYLE_ASSIGNMENT (( #4359 ) ) ;
#4652 = CARTESIAN_POINT ( 'NONE',  ( 0.000000000000000000, 0.000000000000000000, -11.07201791628681775 ) ) ;
#4653 = FACE_OUTER_BOUND ( 'NONE', #53, .T. ) ;
#4654 = VECTOR ( 'NONE', #1289, 1000.000000000000000 ) ;
#4655 = AXIS2_PLACEMENT_3D ( 'NONE', #2320, #5153, #1800 ) ;
#4656 = EDGE_CURVE ( 'NONE', #3300, #2868, #4423, .T. ) ;
#4657 = EDGE_CURVE ( 'NONE', #5234, #3078, #2524, .T. ) ;
#4658 = CIRCLE ( 'NONE', #4490, 14.99999999999998579 ) ;
#4659 = VECTOR ( 'NONE', #3939, 1000.000000000000000 ) ;
#4660 = DIRECTION ( 'NONE',  ( 0.000000000000000000, 0.000000000000000000, 1.000000000000000000 ) ) ;
#4661 = UNCERTAINTY_MEASURE_WITH_UNIT (LENGTH_MEASURE( 1.000000000000000082E-05 ), #4325, 'distance_accuracy_value', 'NONE');
#4662 = DIRECTION ( 'NONE',  ( -0.000000000000000000, 0.8660254037844392627, 0.4999999999999989453 ) ) ;
#4663 = VECTOR ( 'NONE', #3095, 1000.000000000000000 ) ;
#4664 = APPLICATION_CONTEXT ( 'automotive_design' ) ;
#4665 = CARTESIAN_POINT ( 'NONE',  ( 0.6000000000000033085, 0.000000000000000000, 8.400000000000000355 ) ) ;
#4666 = AXIS2_PLACEMENT_3D ( 'NONE', #1155, #4855, #5358 ) ;
#4667 =( NAMED_UNIT ( * ) PLANE_ANGLE_UNIT ( ) SI_UNIT ( $, .RADIAN. ) );
#4668 = CIRCLE ( 'NONE', #4338, 6.499999999999983125 ) ;
#4669 = ORIENTED_EDGE ( 'NONE', *, *, #1686, .F. ) ;
#4670 = DIRECTION ( 'NONE',  ( -1.000000000000000000, -0.000000000000000000, -0.000000000000000000 ) ) ;
#4671 = CARTESIAN_POINT ( 'NONE',  ( -6.499999999999984901, 35.00000000000000000, 30.00000000000000711 ) ) ;
#4672 = AXIS2_PLACEMENT_3D ( 'NONE', #2545, #2150, #3825 ) ;
#4673 = PRODUCT_RELATED_PRODUCT_CATEGORY ( 'part', '', ( #918 ) ) ;
#4674 = LINE ( 'NONE', #895, #4713 ) ;
#4675 = DIRECTION ( 'NONE',  ( 0.000000000000000000, 0.000000000000000000, -1.000000000000000000 ) ) ;
#4676 = CARTESIAN_POINT ( 'NONE',  ( 12.07201791628681420, 0.000000000000000000, -12.00000000000000178 ) ) ;
#4677 = DIRECTION ( 'NONE',  ( 2.081668171172168513E-16, 0.000000000000000000, -1.000000000000000000 ) ) ;
#4678 = ORIENTED_EDGE ( 'NONE', *, *, #3799, .T. ) ;
#4679 = CARTESIAN_POINT ( 'NONE',  ( 9.244715922125777752, -5.337439226220939581, -9.530716183751502868 ) ) ;
#4680 =( LENGTH_UNIT ( ) NAMED_UNIT ( * ) SI_UNIT ( .MILLI., .METRE. ) );
#4681 = EDGE_LOOP ( 'NONE', ( #3724, #5148 ) ) ;
#4682 = CARTESIAN_POINT ( 'NONE',  ( 0.000000000000000000, 10.00000000000000000, 0.000000000000000000 ) ) ;
#4683 = CARTESIAN_POINT ( 'NONE',  ( 0.000000000000000000, 5.839897972853065333, -6.938893903907228378E-15 ) ) ;
#4684 = CARTESIAN_POINT ( 'NONE',  ( 6.000000000000000000, 5.839897972853065333, -6.938893903907228378E-15 ) ) ;
#4685 = CARTESIAN_POINT ( 'NONE',  ( -25.00000000000000000, 60.00000000000000711, 25.00000000000000000 ) ) ;
#4686 = DIRECTION ( 'NONE',  ( -0.000000000000000000, -0.000000000000000000, 1.000000000000000000 ) ) ;
#4687 = EDGE_CURVE ( 'NONE', #1518, #4623, #2386, .T. ) ;
#4688 = CARTESIAN_POINT ( 'NONE',  ( 6.000000000000000000, 5.839897972853065333, -6.938893903907228378E-15 ) ) ;
#4689 = ORIENTED_EDGE ( 'NONE', *, *, #961, .F. ) ;
#4690 = ORIENTED_EDGE ( 'NONE', *, *, #1128, .T. ) ;
#4691 = CARTESIAN_POINT ( 'NONE',  ( -6.000000000000007994, 570.0000000000000000, 30.00000000000001066 ) ) ;
#4692 = CARTESIAN_POINT ( 'NONE',  ( 139.9999999999999716, 885.0000000000000000, 25.00000000000000000 ) ) ;
#4693 = CARTESIAN_POINT ( 'NONE',  ( 0.000000000000000000, 0.000000000000000000, -0.6932054628276118624 ) ) ;
#4694 = EDGE_CURVE ( 'NONE', #3498, #1075, #722, .T. ) ;
#4695 = EDGE_LOOP ( 'NONE', ( #1474, #155, #4052, #1962 ) ) ;
#4696 = DIRECTION ( 'NONE',  ( 1.000000000000000000, 0.000000000000000000, 0.000000000000000000 ) ) ;
#4697 = FACE_BOUND ( 'NONE', #1648, .T. ) ;
#4698 = EDGE_CURVE ( 'NONE', #3352, #3274, #3206, .T. ) ;
#4699 = CARTESIAN_POINT ( 'NONE',  ( -9.000000000000005329, -4.330127018922199866, -8.787392856021028820 ) ) ;
#4700 = CARTESIAN_POINT ( 'NONE',  ( 9.058808647644763568, -5.230105611255016385, -9.269271692759769365 ) ) ;
#4701 = CARTESIAN_POINT ( 'NONE',  ( 0.000000000000000000, 0.000000000000000000, 0.000000000000000000 ) ) ;
#4702 = ORIENTED_EDGE ( 'NONE', *, *, #3425, .F. ) ;
#4703 = CARTESIAN_POINT ( 'NONE',  ( -25.00000000000000000, 60.00000000000000711, -25.00000000000000000 ) ) ;
#4704 = ORIENTED_EDGE ( 'NONE', *, *, #3216, .T. ) ;
#4705 = DIRECTION ( 'NONE',  ( -0.000000000000000000, -0.000000000000000000, 1.000000000000000000 ) ) ;
#4706 = CARTESIAN_POINT ( 'NONE',  ( 139.9999999999999716, 810.0000000000000000, 25.00000000000000000 ) ) ;
#4707 = DIRECTION ( 'NONE',  ( 0.000000000000000000, 0.000000000000000000, -1.000000000000000000 ) ) ;
#4708 = LINE ( 'NONE', #5137, #2959 ) ;
#4709 = DIRECTION ( 'NONE',  ( -0.000000000000000000, -0.000000000000000000, 1.000000000000000000 ) ) ;
#4710 =( NAMED_UNIT ( * ) SI_UNIT ( $, .STERADIAN. ) SOLID_ANGLE_UNIT ( ) );
#4711 = ORIENTED_EDGE ( 'NONE', *, *, #859, .F. ) ;
#4712 = ADVANCED_FACE ( 'NONE', ( #1965 ), #3656, .F. ) ;
#4713 = VECTOR ( 'NONE', #4602, 1000.000000000000000 ) ;
#4714 = VERTEX_POINT ( 'NONE', #5029 ) ;
#4715 = SURFACE_STYLE_FILL_AREA ( #3896 ) ;
#4716 = EDGE_CURVE ( 'NONE', #4283, #656, #523, .T. ) ;
#4717 = DIRECTION ( 'NONE',  ( 0.000000000000000000, 0.000000000000000000, -1.000000000000000000 ) ) ;
#4718 = CARTESIAN_POINT ( 'NONE',  ( 0.000000000000000000, 820.0000000000001137, 6.500000000000000888 ) ) ;
#4719 = VERTEX_POINT ( 'NONE', #2184 ) ;
#4720 = AXIS2_PLACEMENT_3D ( 'NONE', #559, #994, #2045 ) ;
#4721 = EDGE_LOOP ( 'NONE', ( #2871, #1330 ) ) ;
#4722 = ORIENTED_EDGE ( 'NONE', *, *, #2387, .F. ) ;
#4723 = CARTESIAN_POINT ( 'NONE',  ( 91.03600000000004400, 0.000000000000000000, 0.000000000000000000 ) ) ;
#4724 = CARTESIAN_POINT ( 'NONE',  ( 9.473745496805529243, 1.478328004173170497E-13, -9.138786188337405747 ) ) ;
#4725 = DIRECTION ( 'NONE',  ( 0.000000000000000000, 0.000000000000000000, 1.000000000000000000 ) ) ;
#4726 = EDGE_LOOP ( 'NONE', ( #3152, #1565 ) ) ;
#4727 = FACE_BOUND ( 'NONE', #4870, .T. ) ;
#4728 =( NAMED_UNIT ( * ) PLANE_ANGLE_UNIT ( ) SI_UNIT ( $, .RADIAN. ) );
#4729 = CONICAL_SURFACE ( 'NONE', #2494, 9.000000000000001776, 0.8594454914424796144 ) ;
#4730 = STYLED_ITEM ( 'NONE', ( #5320 ), #2946 ) ;
#4731 = EDGE_LOOP ( 'NONE', ( #1297, #5207, #3623, #2670 ) ) ;
#4732=STYLED_ITEM('',(#5426),#47);
#4733 = DIRECTION ( 'NONE',  ( 0.000000000000000000, 0.000000000000000000, 1.000000000000000000 ) ) ;
#4734 = CARTESIAN_POINT ( 'NONE',  ( 121.7157287525384533, 0.000000000000000000, 121.7157287525376859 ) ) ;
#4735 = CARTESIAN_POINT ( 'NONE',  ( 7.347880794884115792E-16, 839.0360000000000582, 5.999999999999996447 ) ) ;
#4736 = CARTESIAN_POINT ( 'NONE',  ( 6.000000000000000000, 2.919948986426538440, 5.057499999999994778 ) ) ;
#4737 = PLANE ( 'NONE',  #3305 ) ;
#4738 = CONICAL_SURFACE ( 'NONE', #2500, 5.036000000000040444, 0.7853981633974339571 ) ;
#4739 = ADVANCED_FACE ( 'NONE', ( #4969 ), #511, .F. ) ;
#4740 = AXIS2_PLACEMENT_3D ( 'NONE', #4162, #2125, #3831 ) ;
#4741 = VECTOR ( 'NONE', #2215, 1000.000000000000000 ) ;
#4742 = CARTESIAN_POINT ( 'NONE',  ( 8.999999999999998224, 5.196152422706628471, -9.106324069981646119 ) ) ;
#4743 = CARTESIAN_POINT ( 'NONE',  ( -150.0000000000000000, 885.0000000000000000, -25.00000000000000000 ) ) ;
#4744 = SHAPE_REPRESENTATION_RELATIONSHIP ( 'NONE' , 'NONE' ,  #3275, #119 ) ;
#4745 = MECHANICAL_DESIGN_GEOMETRIC_PRESENTATION_REPRESENTATION (  '', ( #67 ), #768 ) ;
#4746 = CONICAL_SURFACE ( 'NONE', #1717, 6.000000000000000000, 0.9599310885968784790 ) ;
#4747 = ORIENTED_EDGE ( 'NONE', *, *, #2662, .F. ) ;
#4748 = ORIENTED_EDGE ( 'NONE', *, *, #4327, .F. ) ;
#4749 = CARTESIAN_POINT ( 'NONE',  ( -150.0000000000000284, 0.000000000000000000, 149.9999999999999147 ) ) ;
#4750 = DIRECTION ( 'NONE',  ( -0.000000000000000000, -0.000000000000000000, 1.000000000000000000 ) ) ;
#4751 = EDGE_CURVE ( 'NONE', #5225, #4147, #4552, .T. ) ;
#4752 = CIRCLE ( 'NONE', #5205, 6.499999999999983125 ) ;
#4753 = EDGE_LOOP ( 'NONE', ( #2616, #329, #3213 ) ) ;
#4754 = VERTEX_POINT ( 'NONE', #91 ) ;
#4755 = B_SPLINE_CURVE_WITH_KNOTS ( 'NONE', 3,
 ( #946, #2622, #4231, #3802, #1306, #2984, #3828, #1742, #922, #4260, #131, #1793 ),
 .UNSPECIFIED., .F., .F.,
 ( 4, 2, 2, 2, 2, 4 ),
 ( 0.01261372891313921468, 0.01327902839800527111, 0.01394432788287132755, 0.01527492685260344041, 0.01660552582233554980, 0.01793612479206766266 ),
 .UNSPECIFIED. ) ;
#4756 = CARTESIAN_POINT ( 'NONE',  ( -7.552115898706446728, 6.032088698343841315, -0.5428950306860266251 ) ) ;
#4757 = DIRECTION ( 'NONE',  ( 0.000000000000000000, 0.000000000000000000, -1.000000000000000000 ) ) ;
#4758 = AXIS2_PLACEMENT_3D ( 'NONE', #4875, #1090, #2016 ) ;
#4759 = DIRECTION ( 'NONE',  ( -0.000000000000000000, -1.000000000000000000, -0.000000000000000000 ) ) ;
#4760 = CARTESIAN_POINT ( 'NONE',  ( 6.499999999999981348, 35.00000000000000000, -25.00000000000000000 ) ) ;
#4761 = CARTESIAN_POINT ( 'NONE',  ( 0.000000000000000000, 832.0000000000001137, 0.000000000000000000 ) ) ;
#4762 = CARTESIAN_POINT ( 'NONE',  ( -9.000000000000000000, -5.196152422706636465, -12.00000000000000000 ) ) ;
#4763 = ORIENTED_EDGE ( 'NONE', *, *, #342, .T. ) ;
#4764 = PRESENTATION_STYLE_ASSIGNMENT (( #2738 ) ) ;
#4765 = B_SPLINE_CURVE_WITH_KNOTS ( 'NONE', 3,
 ( #4601, #437, #3797, #2095, #4621, #4645 ),
 .UNSPECIFIED., .F., .F.,
 ( 4, 2, 4 ),
 ( 0.005333245961717304230, 0.007986067645924081054, 0.01063888933013085701 ),
 .UNSPECIFIED. ) ;
#4766 = CARTESIAN_POINT ( 'NONE',  ( -121.7157287525381122, -20.00000000000000000, 136.7157287525380127 ) ) ;
#4767 = CARTESIAN_POINT ( 'NONE',  ( -6.499999999999988454, 330.0000000000000000, -25.00000000000000000 ) ) ;
#4768 = APPLICATION_CONTEXT ( 'automotive_design' ) ;
#4769 = DIRECTION ( 'NONE',  ( -6.938893903907228378E-17, 0.000000000000000000, 1.000000000000000000 ) ) ;
#4770 = ADVANCED_FACE ( 'NONE', ( #3013, #2126 ), #1748, .F. ) ;
#4771 = CARTESIAN_POINT ( 'NONE',  ( 9.477391180807693161, 1.839439615276918794, -9.189449912164228351 ) ) ;
#4772 = CYLINDRICAL_SURFACE ( 'NONE', #1283, 6.499999999999993783 ) ;
#4773 = COLOUR_RGB ( '',0.8941176470588234615, 0.8941176470588234615, 0.8941176470588234615 ) ;
#4774 = ADVANCED_FACE ( 'NONE', ( #4653 ), #3805, .F. ) ;
#4775 = ORIENTED_EDGE ( 'NONE', *, *, #3506, .F. ) ;
#4776 = PRESENTATION_STYLE_ASSIGNMENT (( #5223 ) ) ;
#4777 = ORIENTED_EDGE ( 'NONE', *, *, #609, .T. ) ;
#4778 = CARTESIAN_POINT ( 'NONE',  ( -150.0000000000000284, 10.00000000000000000, -150.0000000000000853 ) ) ;
#4779 = ORIENTED_EDGE ( 'NONE', *, *, #3921, .T. ) ;
#4780 = DIRECTION ( 'NONE',  ( -1.000000000000000000, 0.000000000000000000, 0.000000000000000000 ) ) ;
#4781 = EDGE_CURVE ( 'NONE', #3078, #2509, #1526, .T. ) ;
#4782 = VERTEX_POINT ( 'NONE', #4995 ) ;
#4783 = ORIENTED_EDGE ( 'NONE', *, *, #3699, .F. ) ;
#4784 = CARTESIAN_POINT ( 'NONE',  ( -4.500000000000003553, 7.794228634059947147, 0.000000000000000000 ) ) ;
#4785 = CARTESIAN_POINT ( 'NONE',  ( 121.7157287525372311, -20.00000000000000000, -136.7157287525388085 ) ) ;
#4786 = B_SPLINE_CURVE_WITH_KNOTS ( 'NONE', 3,
 ( #5034, #43, #3813, #1296, #3408, #3458, #96, #3382, #2507, #3763 ),
 .UNSPECIFIED., .F., .F.,
 ( 4, 2, 2, 2, 4 ),
 ( 0.000000000000000000, 0.002766603965071790135, 0.005533207930143580269, 0.008299811895215371271, 0.01106641586028716054 ),
 .UNSPECIFIED. ) ;
#4787 = PLANE ( 'NONE',  #5376 ) ;
#4788 = FACE_OUTER_BOUND ( 'NONE', #4119, .T. ) ;
#4789 = VERTEX_POINT ( 'NONE', #4607 ) ;
#4790 = DIRECTION ( 'NONE',  ( 1.000000000000000000, 0.000000000000000000, 0.000000000000000000 ) ) ;
#4791 = SHAPE_REPRESENTATION ( 'MAS-195', ( #216, #4655, #3020, #2314, #5375, #662, #3731, #1352, #2758, #400, #2131, #4568, #2754 ), #4921 ) ;
#4792 = EDGE_CURVE ( 'NONE', #4918, #4486, #1259, .T. ) ;
#4793 = DIRECTION ( 'NONE',  ( 1.000000000000000000, 0.000000000000000000, 0.000000000000000000 ) ) ;
#4794 = EDGE_LOOP ( 'NONE', ( #1999, #3336, #4187, #4917 ) ) ;
#4795 = CARTESIAN_POINT ( 'NONE',  ( 0.000000000000000000, 10.39230484541326760, -1.199999999999999734 ) ) ;
#4796 = FACE_OUTER_BOUND ( 'NONE', #613, .T. ) ;
#4797 = LINE ( 'NONE', #3941, #857 ) ;
#4798 = DIRECTION ( 'NONE',  ( 0.000000000000000000, 0.8660254037844379305, -0.5000000000000012212 ) ) ;
#4799 = DIRECTION ( 'NONE',  ( -0.000000000000000000, -0.000000000000000000, 1.000000000000000000 ) ) ;
#4800 = EDGE_CURVE ( 'NONE', #4789, #5225, #65, .T. ) ;
#4801 =( NAMED_UNIT ( * ) PLANE_ANGLE_UNIT ( ) SI_UNIT ( $, .RADIAN. ) );
#4802 = ORIENTED_EDGE ( 'NONE', *, *, #1705, .T. ) ;
#4803 = CARTESIAN_POINT ( 'NONE',  ( 137.5000000000000000, 870.0000000000000000, 0.000000000000000000 ) ) ;
#4804 = ORIENTED_EDGE ( 'NONE', *, *, #3438, .F. ) ;
#4805 = DIRECTION ( 'NONE',  ( 0.000000000000000000, 0.000000000000000000, 1.000000000000000000 ) ) ;
#4806 =( NAMED_UNIT ( * ) SI_UNIT ( $, .STERADIAN. ) SOLID_ANGLE_UNIT ( ) );
#4807 = CIRCLE ( 'NONE', #2651, 6.000000000000005329 ) ;
#4808 = EDGE_CURVE ( 'NONE', #871, #3246, #3745, .T. ) ;
#4809 = ORIENTED_EDGE ( 'NONE', *, *, #1736, .F. ) ;
#4810 = ORIENTED_EDGE ( 'NONE', *, *, #2637, .F. ) ;
#4811 = CARTESIAN_POINT ( 'NONE',  ( -9.369866752751233818, 5.409695091966935543, -9.628560800353236360 ) ) ;
#4812 = CARTESIAN_POINT ( 'NONE',  ( -1.538998812064025667, -10.06940755529870302, -9.383905213721176253 ) ) ;
#4813 = CARTESIAN_POINT ( 'NONE',  ( 6.000000000000000000, -2.919948986426526893, 5.057500000000001883 ) ) ;
#4814 = DIRECTION ( 'NONE',  ( -0.5000000000000046629, 0.000000000000000000, 0.8660254037844359321 ) ) ;
#4815 = CIRCLE ( 'NONE', #2210, 6.000000000000001776 ) ;
#4816 = DIRECTION ( 'NONE',  ( 0.9237280213470682178, 0.3830490080632377725, 1.131240564625405124E-16 ) ) ;
#4817 = EDGE_LOOP ( 'NONE', ( #3710, #3975 ) ) ;
#4818 = ORIENTED_EDGE ( 'NONE', *, *, #938, .T. ) ;
#4819 = CIRCLE ( 'NONE', #2661, 5.999999999999993783 ) ;
#4820 = DIRECTION ( 'NONE',  ( 0.000000000000000000, 0.000000000000000000, 1.000000000000000000 ) ) ;
#4821 = FACE_BOUND ( 'NONE', #577, .T. ) ;
#4822 = FILL_AREA_STYLE_COLOUR ( '', #3893 ) ;
#4823 = DIRECTION ( 'NONE',  ( 0.000000000000000000, 0.000000000000000000, 1.000000000000000000 ) ) ;
#4824 = CARTESIAN_POINT ( 'NONE',  ( -2.999999999999998668, -8.660254037844394404, -8.505011083697297636 ) ) ;
#4825 = AXIS2_PLACEMENT_3D ( 'NONE', #3511, #5226, #3950 ) ;
#4826 = ADVANCED_FACE ( 'NONE', ( #4727, #4788 ), #2626, .T. ) ;
#4827 = ADVANCED_FACE ( 'NONE', ( #544, #5129 ), #1008, .F. ) ;
#4828 = EDGE_CURVE ( 'NONE', #4946, #1196, #3908, .T. ) ;
#4829 = MECHANICAL_DESIGN_GEOMETRIC_PRESENTATION_REPRESENTATION (  '', ( #3627 ), #401 ) ;
#4830 = CARTESIAN_POINT ( 'NONE',  ( 9.000000000000000000, -5.581221688749905319, -9.543752152530549537 ) ) ;
#4831 = CARTESIAN_POINT ( 'NONE',  ( 0.000000000000000000, 10.00000000000000000, -30.00000000000000355 ) ) ;
#4832 = VERTEX_POINT ( 'NONE', #1872 ) ;
#4833 = VERTEX_POINT ( 'NONE', #3880 ) ;
#4834 = CIRCLE ( 'NONE', #5284, 5.057500000000000107 ) ;
#4835 = ORIENTED_EDGE ( 'NONE', *, *, #4716, .T. ) ;
#4836 = SURFACE_STYLE_USAGE ( .BOTH. , #2366 ) ;
#4837 = FACE_OUTER_BOUND ( 'NONE', #4514, .T. ) ;
#4838 = ORIENTED_EDGE ( 'NONE', *, *, #2265, .F. ) ;
#4839 = CARTESIAN_POINT ( 'NONE',  ( -30.00000000000000355, 610.0000000000000000, 30.00000000000000000 ) ) ;
#4840 = AXIS2_PLACEMENT_3D ( 'NONE', #1988, #5297, #3671 ) ;
#4841 = CONICAL_SURFACE ( 'NONE', #1975, 9.000000000000001776, 0.8594454914424796144 ) ;
#4842 = APPLICATION_CONTEXT ( 'automotive_design' ) ;
#4843 = ORIENTED_EDGE ( 'NONE', *, *, #2283, .T. ) ;
#4844 = DIRECTION ( 'NONE',  ( 0.5000000000000004441, 0.8660254037844384856, -0.000000000000000000 ) ) ;
#4845 = DIRECTION ( 'NONE',  ( -1.000000000000000000, 0.000000000000000000, 0.000000000000000000 ) ) ;
#4846 = CARTESIAN_POINT ( 'NONE',  ( -137.5000000000000000, 870.0000000000000000, 0.000000000000000000 ) ) ;
#4847 = LINE ( 'NONE', #3609, #4095 ) ;
#4848 = CIRCLE ( 'NONE', #2152, 0.5999999999999998668 ) ;
#4849 = APPLICATION_PROTOCOL_DEFINITION ( 'draft international standard', 'automotive_design', 1998, #2921 ) ;
#4850 = CIRCLE ( 'NONE', #423, 6.499999999999988454 ) ;
#4851 = FACE_BOUND ( 'NONE', #4525, .T. ) ;
#4852 = ORIENTED_EDGE ( 'NONE', *, *, #940, .T. ) ;
#4853 =( LENGTH_UNIT ( ) NAMED_UNIT ( * ) SI_UNIT ( .MILLI., .METRE. ) );
#4854 = DIRECTION ( 'NONE',  ( 0.000000000000000000, 0.000000000000000000, -1.000000000000000000 ) ) ;
#4855 = DIRECTION ( 'NONE',  ( -1.000000000000000000, -0.000000000000000000, -0.000000000000000000 ) ) ;
#4856 = EDGE_CURVE ( 'NONE', #5257, #838, #1369, .T. ) ;
#4857 = EDGE_CURVE ( 'NONE', #2752, #3572, #186, .T. ) ;
#4858 = CARTESIAN_POINT ( 'NONE',  ( -137.5000000000000000, 870.0000000000000000, 0.000000000000000000 ) ) ;
#4859 = DIRECTION ( 'NONE',  ( 0.000000000000000000, 0.000000000000000000, 1.000000000000000000 ) ) ;
#4860 = ORIENTED_EDGE ( 'NONE', *, *, #829, .F. ) ;
#4861 = ORIENTED_EDGE ( 'NONE', *, *, #4237, .F. ) ;
#4862 = FACE_BOUND ( 'NONE', #3083, .T. ) ;
#4863 = FACE_OUTER_BOUND ( 'NONE', #3223, .T. ) ;
#4864 = ORIENTED_EDGE ( 'NONE', *, *, #4828, .F. ) ;
#4865 = FACE_BOUND ( 'NONE', #1995, .T. ) ;
#4866 =( GEOMETRIC_REPRESENTATION_CONTEXT ( 3 ) GLOBAL_UNCERTAINTY_ASSIGNED_CONTEXT ( ( #4442 ) ) GLOBAL_UNIT_ASSIGNED_CONTEXT ( ( #1465, #1553, #1963 ) ) REPRESENTATION_CONTEXT ( 'NONE', 'WORKASPACE' ) );
#4867 = DIRECTION ( 'NONE',  ( 0.000000000000000000, -1.000000000000000000, 0.000000000000000000 ) ) ;
#4868 = EDGE_LOOP ( 'NONE', ( #5168, #1520 ) ) ;
#4869=STYLED_ITEM('',(#5440),#258);
#4870 = EDGE_LOOP ( 'NONE', ( #883, #1108 ) ) ;
#4871 = VERTEX_POINT ( 'NONE', #598 ) ;
#4872 = DIRECTION ( 'NONE',  ( 1.000000000000000000, 0.000000000000000000, 0.000000000000000000 ) ) ;
#4873 = CARTESIAN_POINT ( 'NONE',  ( 5.284168072928040694, 7.341488986065032307, 1.982057096575062005E-15 ) ) ;
#4874 = PLANE ( 'NONE',  #5191 ) ;
#4875 = CARTESIAN_POINT ( 'NONE',  ( -137.5000000000000000, 870.0000000000000000, 0.000000000000000000 ) ) ;
#4876 = UNCERTAINTY_MEASURE_WITH_UNIT (LENGTH_MEASURE( 1.000000000000000082E-05 ), #2048, 'distance_accuracy_value', 'NONE');
#4877 = PRODUCT_CONTEXT ( 'NONE', #5230, 'mechanical' ) ;
#4878 = EDGE_CURVE ( 'NONE', #1204, #2454, #3115, .T. ) ;
#4879 = EDGE_CURVE ( 'NONE', #4553, #2728, #1542, .T. ) ;
#4880 = PLANE ( 'NONE',  #304 ) ;
#4881 = ORIENTED_EDGE ( 'NONE', *, *, #1832, .F. ) ;
#4882 = CARTESIAN_POINT ( 'NONE',  ( 0.000000000000000000, 0.000000000000000000, 0.000000000000000000 ) ) ;
#4883 = DIRECTION ( 'NONE',  ( 0.000000000000000000, 0.000000000000000000, 1.000000000000000000 ) ) ;
#4884 = CARTESIAN_POINT ( 'NONE',  ( -4.500000000000003553, 7.794228634059947147, 0.000000000000000000 ) ) ;
#4885 = CARTESIAN_POINT ( 'NONE',  ( -9.000000000000000000, -5.196152422706636465, -8.935996291721336249 ) ) ;
#4886 = ORIENTED_EDGE ( 'NONE', *, *, #2974, .T. ) ;
#4887 = EDGE_CURVE ( 'NONE', #2372, #508, #108, .T. ) ;
#4888 = ORIENTED_EDGE ( 'NONE', *, *, #2069, .T. ) ;
#4889 = DIRECTION ( 'NONE',  ( -0.000000000000000000, -0.000000000000000000, 1.000000000000000000 ) ) ;
#4890 = FACE_OUTER_BOUND ( 'NONE', #4117, .T. ) ;
#4891 = VERTEX_POINT ( 'NONE', #1402 ) ;
#4892 = EDGE_LOOP ( 'NONE', ( #5341, #3132, #4907, #4516 ) ) ;
#4893 = DIRECTION ( 'NONE',  ( 0.000000000000000000, -1.000000000000000000, 0.000000000000000000 ) ) ;
#4894 = ORIENTED_EDGE ( 'NONE', *, *, #3142, .F. ) ;
#4895 = DIRECTION ( 'NONE',  ( 1.000000000000000000, 0.000000000000000000, 0.000000000000000000 ) ) ;
#4896 = ADVANCED_FACE ( 'NONE', ( #1799 ), #3478, .F. ) ;
#4897 = EDGE_CURVE ( 'NONE', #2509, #5361, #1139, .T. ) ;
#4898 = VERTEX_POINT ( 'NONE', #3933 ) ;
#4899 = CARTESIAN_POINT ( 'NONE',  ( -12.38940648156203927, 0.000000000000000000, -10.20000000000000107 ) ) ;
#4900 = CARTESIAN_POINT ( 'NONE',  ( -150.0000000000000000, 870.0000000000000000, 6.000000000000005329 ) ) ;
#4901 = CARTESIAN_POINT ( 'NONE',  ( 149.9999999999999716, 10.00000000000000000, 149.9999999999999716 ) ) ;
#4902 = DIRECTION ( 'NONE',  ( 0.000000000000000000, -0.000000000000000000, 1.000000000000000000 ) ) ;
#4903 = APPLICATION_PROTOCOL_DEFINITION ( 'draft international standard', 'automotive_design', 1998, #788 ) ;
#4904 = CIRCLE ( 'NONE', #2736, 5.999999999999950262 ) ;
#4905 = CARTESIAN_POINT ( 'NONE',  ( 25.00000000000000000, 210.0000000000000284, -25.00000000000000000 ) ) ;
#4906 = AXIS2_PLACEMENT_3D ( 'NONE', #2572, #538, #3398 ) ;
#4907 = ORIENTED_EDGE ( 'NONE', *, *, #4473, .F. ) ;
#4908 = LINE ( 'NONE', #2020, #5064 ) ;
#4909 = CARTESIAN_POINT ( 'NONE',  ( -139.9999999999999716, 885.0000000000000000, 25.00000000000000000 ) ) ;
#4910 = DIRECTION ( 'NONE',  ( -1.000000000000000000, -0.000000000000000000, -0.000000000000000000 ) ) ;
#4911 = DIRECTION ( 'NONE',  ( 0.000000000000000000, 0.000000000000000000, 1.000000000000000000 ) ) ;
#4912=STYLED_ITEM('',(#5412),#1812);
#4913 = EDGE_LOOP ( 'NONE', ( #1857, #3929, #5119 ) ) ;
#4914 = CARTESIAN_POINT ( 'NONE',  ( 9.370348127518923320, 5.409973013828315302, -9.628763110917944346 ) ) ;
#4915 = FACE_OUTER_BOUND ( 'NONE', #869, .T. ) ;
#4916 =( GEOMETRIC_REPRESENTATION_CONTEXT ( 3 ) GLOBAL_UNCERTAINTY_ASSIGNED_CONTEXT ( ( #2377 ) ) GLOBAL_UNIT_ASSIGNED_CONTEXT ( ( #1538, #704, #178 ) ) REPRESENTATION_CONTEXT ( 'NONE', 'WORKASPACE' ) );
#4917 = ORIENTED_EDGE ( 'NONE', *, *, #5224, .T. ) ;
#4918 = VERTEX_POINT ( 'NONE', #1844 ) ;
#4919 = EDGE_LOOP ( 'NONE', ( #169, #1054, #445, #4035 ) ) ;
#4920 = PRODUCT_DEFINITION ( 'UNKNOWN', '', #1863, #5334 ) ;
#4921 =( GEOMETRIC_REPRESENTATION_CONTEXT ( 3 ) GLOBAL_UNCERTAINTY_ASSIGNED_CONTEXT ( ( #958 ) ) GLOBAL_UNIT_ASSIGNED_CONTEXT ( ( #2410, #3646, #5327 ) ) REPRESENTATION_CONTEXT ( 'NONE', 'WORKASPACE' ) );
#4922 = AXIS2_PLACEMENT_3D ( 'NONE', #2950, #73, #2611 ) ;
#4923 = B_SPLINE_CURVE_WITH_KNOTS ( 'NONE', 3,
 ( #1524, #5335, #5309, #4471, #1100, #4885 ),
 .UNSPECIFIED., .F., .F.,
 ( 4, 2, 4 ),
 ( -5.636559625663623135E-06, 0.0004989239064927824966, 0.001003484372611228564 ),
 .UNSPECIFIED. ) ;
#4924 = CARTESIAN_POINT ( 'NONE',  ( -6.000000000000000000, 0.000000000000000000, -11.97459999999999880 ) ) ;
#4925 = ORIENTED_EDGE ( 'NONE', *, *, #3449, .F. ) ;
#4926 = CONICAL_SURFACE ( 'NONE', #3978, 5.035999999999999588, 0.7853981633974743692 ) ;
#4927 = VECTOR ( 'NONE', #1823, 1000.000000000000000 ) ;
#4928 = VECTOR ( 'NONE', #3146, 1000.000000000000114 ) ;
#4929 = VERTEX_POINT ( 'NONE', #2238 ) ;
#4930 = CARTESIAN_POINT ( 'NONE',  ( 25.00000000000000355, 60.00000000000000711, 25.00000000000000000 ) ) ;
#4931 = EDGE_CURVE ( 'NONE', #3733, #4457, #1063, .T. ) ;
#4932 = DIRECTION ( 'NONE',  ( 0.000000000000000000, 0.000000000000000000, 1.000000000000000000 ) ) ;
#4933 = DIRECTION ( 'NONE',  ( 1.000000000000000000, 0.000000000000000000, 0.000000000000000000 ) ) ;
#4934 = DIRECTION ( 'NONE',  ( -1.000000000000000000, -0.000000000000000000, -0.000000000000000000 ) ) ;
#4935 = UNCERTAINTY_MEASURE_WITH_UNIT (LENGTH_MEASURE( 1.000000000000000082E-05 ), #4853, 'distance_accuracy_value', 'NONE');
#4936 = SHAPE_DEFINITION_REPRESENTATION ( #1354, #3706 ) ;
#4937 = VECTOR ( 'NONE', #8, 1000.000000000000000 ) ;
#4938 = DIRECTION ( 'NONE',  ( 1.000000000000000000, 0.000000000000000000, 0.000000000000000000 ) ) ;
#4939 = ORIENTED_EDGE ( 'NONE', *, *, #3751, .F. ) ;
#4940 = CARTESIAN_POINT ( 'NONE',  ( 6.000000000000000000, -2.919948986426526893, 5.057500000000001883 ) ) ;
#4941 =( NAMED_UNIT ( * ) SI_UNIT ( $, .STERADIAN. ) SOLID_ANGLE_UNIT ( ) );
#4942 = PLANE ( 'NONE',  #661 ) ;
#4943 = CARTESIAN_POINT ( 'NONE',  ( 150.0000000000000000, 810.0000000000000000, -25.00000000000000000 ) ) ;
#4944 = ORIENTED_EDGE ( 'NONE', *, *, #3260, .T. ) ;
#4945 = AXIS2_PLACEMENT_3D ( 'NONE', #3582, #2376, #357 ) ;
#4946 = VERTEX_POINT ( 'NONE', #3522 ) ;
#4947 = DIRECTION ( 'NONE',  ( -0.000000000000000000, -1.000000000000000000, -0.000000000000000000 ) ) ;
#4948 = PLANE ( 'NONE',  #3633 ) ;
#4949 = CIRCLE ( 'NONE', #1448, 6.499999999999988454 ) ;
#4950 = ORIENTED_EDGE ( 'NONE', *, *, #4808, .F. ) ;
#4951 = VERTEX_POINT ( 'NONE', #4760 ) ;
#4952 = ORIENTED_EDGE ( 'NONE', *, *, #69, .F. ) ;
#4953 = EDGE_CURVE ( 'NONE', #4122, #3640, #1042, .T. ) ;
#4954 = ADVANCED_FACE ( 'NONE', ( #2290 ), #3553, .F. ) ;
#4955 = CARTESIAN_POINT ( 'NONE',  ( 0.000000000000000000, 839.0360000000000582, 0.000000000000000000 ) ) ;
#4956 = ORIENTED_EDGE ( 'NONE', *, *, #2305, .F. ) ;
#4957 = ORIENTED_EDGE ( 'NONE', *, *, #352, .T. ) ;
#4958 = APPLICATION_CONTEXT ( 'automotive_design' ) ;
#4959 = VERTEX_POINT ( 'NONE', #1515 ) ;
#4960 = CARTESIAN_POINT ( 'NONE',  ( 12.59999999999999964, 0.000000000000000000, 0.000000000000000000 ) ) ;
#4961 = CARTESIAN_POINT ( 'NONE',  ( -137.5000000000000000, 870.0000000000000000, 6.000000000000006217 ) ) ;
#4962 = CARTESIAN_POINT ( 'NONE',  ( -9.000000000000000000, -3.085342593989932158, -0.4353033105082920184 ) ) ;
#4963 = EDGE_CURVE ( 'NONE', #3270, #1147, #2885, .T. ) ;
#4964 =( NAMED_UNIT ( * ) PLANE_ANGLE_UNIT ( ) SI_UNIT ( $, .RADIAN. ) );
#4965 = VERTEX_POINT ( 'NONE', #4522 ) ;
#4966 = DIRECTION ( 'NONE',  ( 0.000000000000000000, 0.000000000000000000, 1.000000000000000000 ) ) ;
#4967 = FILL_AREA_STYLE ('',( #4822 ) ) ;
#4968 = CARTESIAN_POINT ( 'NONE',  ( 6.000000000000000000, 4.379923479639800554, 2.528749999999996056 ) ) ;
#4969 = FACE_OUTER_BOUND ( 'NONE', #3239, .T. ) ;
#4970 = EDGE_LOOP ( 'NONE', ( #1566, #2931 ) ) ;
#4971 = PRODUCT ( 'main roller', 'main roller', '', ( #2887 ) ) ;
#4972 = EDGE_CURVE ( 'NONE', #2954, #4951, #4752, .T. ) ;
#4973 = EDGE_CURVE ( 'NONE', #4782, #1075, #2694, .T. ) ;
#4974 = EDGE_LOOP ( 'NONE', ( #878, #4299, #197, #3143, #1357, #2088, #2070, #2724 ) ) ;
#4975 = EDGE_CURVE ( 'NONE', #4623, #5043, #800, .T. ) ;
#4976 = DIRECTION ( 'NONE',  ( -0.000000000000000000, -0.000000000000000000, 1.000000000000000000 ) ) ;
#4977 = CARTESIAN_POINT ( 'NONE',  ( -150.0000000000000000, 810.0000000000000000, 25.00000000000000000 ) ) ;
#4978 = ORIENTED_EDGE ( 'NONE', *, *, #2811, .T. ) ;
#4979 = ORIENTED_EDGE ( 'NONE', *, *, #593, .T. ) ;
#4980 = DIRECTION ( 'NONE',  ( -0.000000000000000000, -0.000000000000000000, 1.000000000000000000 ) ) ;
#4981 = EDGE_CURVE ( 'NONE', #5200, #1279, #3998, .T. ) ;
#4982 = VERTEX_POINT ( 'NONE', #271 ) ;
#4983 = ORIENTED_EDGE ( 'NONE', *, *, #2561, .T. ) ;
#4984 = PRESENTATION_STYLE_ASSIGNMENT (( #3770 ) ) ;
#4985 = EDGE_LOOP ( 'NONE', ( #3764, #5055 ) ) ;
#4986 = ORIENTED_EDGE ( 'NONE', *, *, #787, .F. ) ;
#4987 = FACE_OUTER_BOUND ( 'NONE', #1947, .T. ) ;
#4988 = CARTESIAN_POINT ( 'NONE',  ( -9.417977369734735760, 4.954833075775106010, -9.021743230619930998 ) ) ;
#4989 = FACE_OUTER_BOUND ( 'NONE', #2276, .T. ) ;
#4990 = EDGE_CURVE ( 'NONE', #4507, #2324, #509, .T. ) ;
#4991 = ORIENTED_EDGE ( 'NONE', *, *, #115, .T. ) ;
#4992 = CARTESIAN_POINT ( 'NONE',  ( -1.676835913137321903E-15, 35.00000000000000000, -25.00000000000000000 ) ) ;
#4993 =( LENGTH_UNIT ( ) NAMED_UNIT ( * ) SI_UNIT ( .MILLI., .METRE. ) );
#4994 = CARTESIAN_POINT ( 'NONE',  ( -121.7157287525381122, -20.00000000000000000, 136.7157287525380127 ) ) ;
#4995 = CARTESIAN_POINT ( 'NONE',  ( 6.499999999999988454, 570.0000000000000000, 30.00000000000000711 ) ) ;
#4996 = AXIS2_PLACEMENT_3D ( 'NONE', #4618, #84, #944 ) ;
#4997 =( NAMED_UNIT ( * ) SI_UNIT ( $, .STERADIAN. ) SOLID_ANGLE_UNIT ( ) );
#4998 = CIRCLE ( 'NONE', #1166, 14.99999999999998579 ) ;
#4999 = ORIENTED_EDGE ( 'NONE', *, *, #1718, .T. ) ;
#5000 = ORIENTED_EDGE ( 'NONE', *, *, #2621, .F. ) ;
#5001 = LINE ( 'NONE', #1264, #4570 ) ;
#5002 = CARTESIAN_POINT ( 'NONE',  ( 139.9999999999999716, 820.0000000000001137, 25.00000000000000000 ) ) ;
#5003 = EDGE_LOOP ( 'NONE', ( #3845, #3256, #690, #1230, #2277 ) ) ;
#5004 = AXIS2_PLACEMENT_3D ( 'NONE', #4198, #459, #3795 ) ;
#5005 = ORIENTED_EDGE ( 'NONE', *, *, #4297, .F. ) ;
#5006 = EDGE_CURVE ( 'NONE', #1489, #3274, #4847, .T. ) ;
#5007 = EDGE_CURVE ( 'NONE', #4898, #4535, #76, .T. ) ;
#5008 = AXIS2_PLACEMENT_3D ( 'NONE', #5352, #1213, #804 ) ;
#5009 = DIRECTION ( 'NONE',  ( 0.000000000000000000, 0.000000000000000000, 1.000000000000000000 ) ) ;
#5010 = ORIENTED_EDGE ( 'NONE', *, *, #4237, .T. ) ;
#5011 = SURFACE_STYLE_FILL_AREA ( #845 ) ;
#5012 = VECTOR ( 'NONE', #2701, 1000.000000000000000 ) ;
#5013 =( GEOMETRIC_REPRESENTATION_CONTEXT ( 3 ) GLOBAL_UNCERTAINTY_ASSIGNED_CONTEXT ( ( #4661 ) ) GLOBAL_UNIT_ASSIGNED_CONTEXT ( ( #4325, #4667, #3023 ) ) REPRESENTATION_CONTEXT ( 'NONE', 'WORKASPACE' ) );
#5014 = AXIS2_PLACEMENT_3D ( 'NONE', #4586, #4484, #4068 ) ;
#5015 = ORIENTED_EDGE ( 'NONE', *, *, #2847, .F. ) ;
#5016 = AXIS2_PLACEMENT_3D ( 'NONE', #1849, #1409, #253 ) ;
#5017 = CARTESIAN_POINT ( 'NONE',  ( 12.59999999999999964, 0.000000000000000000, 0.000000000000000000 ) ) ;
#5018 = CARTESIAN_POINT ( 'NONE',  ( -30.00000000000000000, 610.0000000000000000, -30.00000000000000355 ) ) ;
#5019 = STYLED_ITEM ( 'NONE', ( #2992 ), #2208 ) ;
#5020 = CARTESIAN_POINT ( 'NONE',  ( -9.000000000000001776, 0.000000000000000000, 0.000000000000000000 ) ) ;
#5021 = PRODUCT_DEFINITION_SHAPE ( 'NONE', 'NONE',  #5255 ) ;
#5022 = ITEM_DEFINED_TRANSFORMATION ( 'NONE', 'NONE', #2754,  #4154 ) ;
#5023=STYLED_ITEM('',(#5440),#3628);
#5024 = DIRECTION ( 'NONE',  ( 0.000000000000000000, 0.4999999999999990008, -0.8660254037844392627 ) ) ;
#5025 = DIRECTION ( 'NONE',  ( 0.000000000000000000, 1.000000000000000000, -1.188187522481193495E-15 ) ) ;
#5026 = CARTESIAN_POINT ( 'NONE',  ( -2.947989941763851984, -8.690282058967598644, -0.1432599722966032829 ) ) ;
#5027 = EDGE_CURVE ( 'NONE', #838, #5257, #4850, .T. ) ;
#5028 = PLANE ( 'NONE',  #1425 ) ;
#5029 = CARTESIAN_POINT ( 'NONE',  ( -121.7157287525392917, 0.000000000000000000, -136.7157287525368474 ) ) ;
#5030 = CIRCLE ( 'NONE', #2679, 6.499999999999983125 ) ;
#5031 =( LENGTH_UNIT ( ) NAMED_UNIT ( * ) SI_UNIT ( .MILLI., .METRE. ) );
#5032 = ORIENTED_EDGE ( 'NONE', *, *, #3700, .F. ) ;
#5033 = CARTESIAN_POINT ( 'NONE',  ( 6.177322775498883978, 6.825825878107829148, -8.969375302471100042 ) ) ;
#5034 = CARTESIAN_POINT ( 'NONE',  ( 9.506737344437272696, -5.488717364925930653, -9.686084310752812954 ) ) ;
#5035 = ORIENTED_EDGE ( 'NONE', *, *, #4953, .T. ) ;
#5036 = ORIENTED_EDGE ( 'NONE', *, *, #2727, .F. ) ;
#5037 = VECTOR ( 'NONE', #2778, 1000.000000000000000 ) ;
#5038 = ORIENTED_EDGE ( 'NONE', *, *, #2637, .T. ) ;
#5039 = EDGE_CURVE ( 'NONE', #3015, #1224, #336, .T. ) ;
#5040 = VECTOR ( 'NONE', #1768, 1000.000000000000000 ) ;
#5041 = DIRECTION ( 'NONE',  ( -0.000000000000000000, -1.000000000000000000, -0.000000000000000000 ) ) ;
#5042 = VERTEX_POINT ( 'NONE', #3672 ) ;
#5043 = VERTEX_POINT ( 'NONE', #686 ) ;
#5044 = CARTESIAN_POINT ( 'NONE',  ( -6.499999999999988454, 570.0000000000000000, 30.00000000000000711 ) ) ;
#5045 = CARTESIAN_POINT ( 'NONE',  ( -6.106276769875783828, 6.866844308578849976, -9.019248292997451344 ) ) ;
#5046 = CARTESIAN_POINT ( 'NONE',  ( 8.534985340083734329, -5.464628761784584121, -9.367146555587263279 ) ) ;
#5047 = FACE_OUTER_BOUND ( 'NONE', #1307, .T. ) ;
#5048 = CARTESIAN_POINT ( 'NONE',  ( 150.0000000000000000, 810.0000000000000000, -25.00000000000000000 ) ) ;
#5049 = LINE ( 'NONE', #2942, #3287 ) ;
#5050 = EDGE_CURVE ( 'NONE', #1447, #3267, #2350, .T. ) ;
#5051 = ORIENTED_EDGE ( 'NONE', *, *, #631, .F. ) ;
#5052 = CARTESIAN_POINT ( 'NONE',  ( -9.489874121516242766, 3.747692455480259532, -9.361141881131302966 ) ) ;
#5053 = AXIS2_PLACEMENT_3D ( 'NONE', #2383, #3652, #1097 ) ;
#5054 = EDGE_CURVE ( 'NONE', #4929, #2539, #1637, .T. ) ;
#5055 = ORIENTED_EDGE ( 'NONE', *, *, #4038, .F. ) ;
#5056 = ORIENTED_EDGE ( 'NONE', *, *, #2449, .F. ) ;
#5057 = CARTESIAN_POINT ( 'NONE',  ( 0.000000000000000000, 0.000000000000000000, -11.34441321561125626 ) ) ;
#5058 = UNCERTAINTY_MEASURE_WITH_UNIT (LENGTH_MEASURE( 1.000000000000000082E-05 ), #2393, 'distance_accuracy_value', 'NONE');
#5059 = LINE ( 'NONE', #4170, #1110 ) ;
#5060 = EDGE_CURVE ( 'NONE', #4239, #2365, #3905, .T. ) ;
#5061 = APPLICATION_CONTEXT ( 'automotive_design' ) ;
#5062 = CARTESIAN_POINT ( 'NONE',  ( 8.281895533831889367, -5.610750229555068636, -0.8426663529491329463 ) ) ;
#5063 = VERTEX_POINT ( 'NONE', #2851 ) ;
#5064 = VECTOR ( 'NONE', #2821, 1000.000000000000000 ) ;
#5065 = ORIENTED_EDGE ( 'NONE', *, *, #938, .F. ) ;
#5066 = CARTESIAN_POINT ( 'NONE',  ( -9.473745496805529243, -1.478735707944909295E-13, -9.138786188337405747 ) ) ;
#5067 = DIRECTION ( 'NONE',  ( 0.000000000000000000, 0.000000000000000000, -1.000000000000000000 ) ) ;
#5068 = LINE ( 'NONE', #1887, #327 ) ;
#5069 = CARTESIAN_POINT ( 'NONE',  ( 9.334923259264868989, -5.002784388812196781, -9.544071379897776097 ) ) ;
#5070 = ITEM_DEFINED_TRANSFORMATION ( 'NONE', 'NONE', #5375,  #4154 ) ;
#5071 = EDGE_CURVE ( 'NONE', #4512, #2280, #4496, .T. ) ;
#5072 = EDGE_CURVE ( 'NONE', #4832, #1591, #4668, .T. ) ;
#5073 = CARTESIAN_POINT ( 'NONE',  ( 0.000000000000000000, 0.000000000000000000, -0.6932054628276118624 ) ) ;
#5074 = DIRECTION ( 'NONE',  ( 0.000000000000000000, 0.000000000000000000, -1.000000000000000000 ) ) ;
#5075 = DIRECTION ( 'NONE',  ( -0.000000000000000000, -0.000000000000000000, 1.000000000000000000 ) ) ;
#5076 = CARTESIAN_POINT ( 'NONE',  ( -25.00000000000000000, 810.0000000000000000, 24.99999999999999645 ) ) ;
#5077 = EDGE_LOOP ( 'NONE', ( #5102, #1350, #2477 ) ) ;
#5078 = CARTESIAN_POINT ( 'NONE',  ( -9.507374272674303128, -5.554564088132607047, -9.698321345470532151 ) ) ;
#5079 = EDGE_LOOP ( 'NONE', ( #374, #427, #1027, #2247 ) ) ;
#5080 = FILL_AREA_STYLE ('',( #504 ) ) ;
#5081 = CARTESIAN_POINT ( 'NONE',  ( 2.865539685210587439, 8.737884736783376738, -8.512883888440002877 ) ) ;
#5082 = DIRECTION ( 'NONE',  ( 1.000000000000000000, 0.000000000000000000, 0.000000000000000000 ) ) ;
#5083 = AXIS2_PLACEMENT_3D ( 'NONE', #3606, #1004, #4383 ) ;
#5084 = CARTESIAN_POINT ( 'NONE',  ( 137.5000000000000000, 870.0000000000000000, 20.00000000000001421 ) ) ;
#5085 = CONICAL_SURFACE ( 'NONE', #4055, 9.000000000000001776, 0.8594454914424796144 ) ;
#5086 = FILL_AREA_STYLE ('',( #5116 ) ) ;
#5087 = AXIS2_PLACEMENT_3D ( 'NONE', #1015, #600, #275 ) ;
#5088 = ORIENTED_EDGE ( 'NONE', *, *, #1177, .F. ) ;
#5089 = DIRECTION ( 'NONE',  ( 0.000000000000000000, 0.000000000000000000, -1.000000000000000000 ) ) ;
#5090 = FACE_BOUND ( 'NONE', #5345, .T. ) ;
#5091 = CARTESIAN_POINT ( 'NONE',  ( 6.000000000000000000, 5.839897972853065333, -6.938893903907228378E-15 ) ) ;
#5092 = VECTOR ( 'NONE', #4269, 1000.000000000000000 ) ;
#5093 = CLOSED_SHELL ( 'NONE', ( #4362, #2581, #408, #452, #223, #4896, #3346, #2051, #1926, #2391, #1331, #930, #2493, #3723, #237, #4314, #3782, #4499, #3855, #543, #5206 ) ) ;
#5094 = ORIENTED_EDGE ( 'NONE', *, *, #2030, .F. ) ;
#5095 = AXIS2_PLACEMENT_3D ( 'NONE', #2777, #4425, #699 ) ;
#5096 = ADVANCED_FACE ( 'NONE', ( #4048 ), #1953, .F. ) ;
#5097 = PRESENTATION_LAYER_ASSIGNMENT (  '', '', ( #910 ) ) ;
#5098 = FACE_OUTER_BOUND ( 'NONE', #1187, .T. ) ;
#5099 = DIRECTION ( 'NONE',  ( 0.000000000000000000, -0.000000000000000000, 1.000000000000000000 ) ) ;
#5100 = DIRECTION ( 'NONE',  ( 0.000000000000000000, 1.000000000000000000, 0.000000000000000000 ) ) ;
#5101 = DIRECTION ( 'NONE',  ( -0.000000000000000000, -1.000000000000000000, -0.000000000000000000 ) ) ;
#5102 = ORIENTED_EDGE ( 'NONE', *, *, #1395, .F. ) ;
#5103 = CARTESIAN_POINT ( 'NONE',  ( 6.499999999999988454, 570.0000000000000000, 25.00000000000000000 ) ) ;
#5104 = VECTOR ( 'NONE', #2989, 1000.000000000000000 ) ;
#5105 = EDGE_CURVE ( 'NONE', #5294, #4480, #3212, .T. ) ;
#5106 = FACE_OUTER_BOUND ( 'NONE', #2189, .T. ) ;
#5107 = ORIENTED_EDGE ( 'NONE', *, *, #2237, .F. ) ;
#5108 = LINE ( 'NONE', #1365, #3584 ) ;
#5109 = CARTESIAN_POINT ( 'NONE',  ( 4.500000000000003553, 7.794228634059947147, 0.000000000000000000 ) ) ;
#5110 = CARTESIAN_POINT ( 'NONE',  ( -0.05670911061056357200, 11.01091124578873703, -9.698321917585792207 ) ) ;
#5111 = CARTESIAN_POINT ( 'NONE',  ( 137.5000000000000000, 870.0000000000000000, 0.000000000000000000 ) ) ;
#5112 = VECTOR ( 'NONE', #4199, 1000.000000000000000 ) ;
#5113 = DIRECTION ( 'NONE',  ( 0.000000000000000000, 0.000000000000000000, 1.000000000000000000 ) ) ;
#5114 = CONICAL_SURFACE ( 'NONE', #334, 5.999999999999993783, 0.7853981633974491672 ) ;
#5115 = ADVANCED_FACE ( 'NONE', ( #2408 ), #2178, .F. ) ;
#5116 = FILL_AREA_STYLE_COLOUR ( '', #4648 ) ;
#5117 = AXIS2_PLACEMENT_3D ( 'NONE', #3061, #3037, #2733 ) ;
#5118 = EDGE_CURVE ( 'NONE', #1794, #4086, #689, .T. ) ;
#5119 = ORIENTED_EDGE ( 'NONE', *, *, #2896, .F. ) ;
#5120 = PLANE ( 'NONE',  #4720 ) ;
#5121 = PLANE ( 'NONE',  #4996 ) ;
#5122 = FACE_OUTER_BOUND ( 'NONE', #2973, .T. ) ;
#5123 = CARTESIAN_POINT ( 'NONE',  ( -150.0000000000000000, 885.0000000000000000, 25.00000000000000000 ) ) ;
#5124 = ORIENTED_EDGE ( 'NONE', *, *, #1066, .T. ) ;
#5125 = CARTESIAN_POINT ( 'NONE',  ( -165.0000000000000000, 870.0000000000000000, 0.000000000000000000 ) ) ;
#5126 = CARTESIAN_POINT ( 'NONE',  ( 6.000000000000000000, 0.000000000000000000, 0.000000000000000000 ) ) ;
#5127 = LINE ( 'NONE', #134, #494 ) ;
#5128 = EDGE_LOOP ( 'NONE', ( #1783, #2232, #4925, #99, #954, #2922, #23, #837 ) ) ;
#5129 = FACE_OUTER_BOUND ( 'NONE', #2, .T. ) ;
#5130 =( LENGTH_UNIT ( ) NAMED_UNIT ( * ) SI_UNIT ( .MILLI., .METRE. ) );
#5131 = ORIENTED_EDGE ( 'NONE', *, *, #4341, .T. ) ;
#5132 = LINE ( 'NONE', #2267, #1334 ) ;
#5133 = ORIENTED_EDGE ( 'NONE', *, *, #4963, .T. ) ;
#5134 = DIRECTION ( 'NONE',  ( 1.000000000000000000, 0.000000000000000000, 0.000000000000000000 ) ) ;
#5135 = CARTESIAN_POINT ( 'NONE',  ( -6.499999999999993783, 570.0000000000000000, 25.00000000000000000 ) ) ;
#5136 = LINE ( 'NONE', #4736, #314 ) ;
#5137 = CARTESIAN_POINT ( 'NONE',  ( 6.499999999999988454, 390.0000000000000000, 25.00000000000000000 ) ) ;
#5138 = ADVANCED_FACE ( 'NONE', ( #4989 ), #2912, .F. ) ;
#5139 = EDGE_CURVE ( 'NONE', #2529, #1794, #4765, .T. ) ;
#5140 = ADVANCED_FACE ( 'NONE', ( #4200 ), #2040, .F. ) ;
#5141 = CARTESIAN_POINT ( 'NONE',  ( 9.489861534733870840, 3.701827684609153568, -9.383895017444986664 ) ) ;
#5142 = VERTEX_POINT ( 'NONE', #3316 ) ;
#5143 = EDGE_LOOP ( 'NONE', ( #3571, #2808, #3760, #2352, #2379, #1539, #815 ) ) ;
#5144 = CARTESIAN_POINT ( 'NONE',  ( -9.506737344437272696, 5.488717364925923548, -9.686084310752812954 ) ) ;
#5145 = CARTESIAN_POINT ( 'NONE',  ( 6.000000000000000000, 0.000000000000000000, 0.000000000000000000 ) ) ;
#5146 = CARTESIAN_POINT ( 'NONE',  ( -9.000000000000000000, 5.196152422706629359, -8.935996291721334472 ) ) ;
#5147 = ORIENTED_EDGE ( 'NONE', *, *, #1528, .T. ) ;
#5148 = ORIENTED_EDGE ( 'NONE', *, *, #2876, .T. ) ;
#5149 = CARTESIAN_POINT ( 'NONE',  ( 3.040097435540409859E-15, 10.46020835156528683, -9.269265075619310679 ) ) ;
#5150 =( NAMED_UNIT ( * ) SI_UNIT ( $, .STERADIAN. ) SOLID_ANGLE_UNIT ( ) );
#5151 = CARTESIAN_POINT ( 'NONE',  ( -9.000000000000001776, -3.464101615137761048, -8.667800885990210702 ) ) ;
#5152 = DIRECTION ( 'NONE',  ( -0.000000000000000000, -0.000000000000000000, 1.000000000000000000 ) ) ;
#5153 = DIRECTION ( 'NONE',  ( 0.000000000000000000, 0.000000000000000000, 1.000000000000000000 ) ) ;
#5154 = ADVANCED_FACE ( 'NONE', ( #2491 ), #4226, .F. ) ;
#5155 = EDGE_LOOP ( 'NONE', ( #5094, #2565 ) ) ;
#5156 = CARTESIAN_POINT ( 'NONE',  ( 30.00000000000000355, 10.00000000000000000, 30.00000000000001066 ) ) ;
#5157 = CARTESIAN_POINT ( 'NONE',  ( 6.000000000000000000, 5.839897972853065333, -6.938893903907228378E-15 ) ) ;
#5158 = DIRECTION ( 'NONE',  ( -0.000000000000000000, -1.000000000000000000, -0.000000000000000000 ) ) ;
#5159 = LINE ( 'NONE', #1441, #4403 ) ;
#5160 = APPLICATION_CONTEXT ( 'automotive_design' ) ;
#5161 = CARTESIAN_POINT ( 'NONE',  ( 137.5000000000000000, 870.0000000000000000, 6.000000000000006217 ) ) ;
#5162 = EDGE_CURVE ( 'NONE', #676, #4719, #57, .T. ) ;
#5163 = CARTESIAN_POINT ( 'NONE',  ( 0.000000000000000000, 820.0000000000001137, 0.000000000000000000 ) ) ;
#5164 = DIRECTION ( 'NONE',  ( 1.000000000000000000, 0.000000000000000000, 2.081668171172168513E-16 ) ) ;
#5165 = ADVANCED_FACE ( 'NONE', ( #1282 ), #874, .F. ) ;
#5166 = CIRCLE ( 'NONE', #290, 9.000000000000001776 ) ;
#5167 = AXIS2_PLACEMENT_3D ( 'NONE', #3952, #1082, #560 ) ;
#5168 = ORIENTED_EDGE ( 'NONE', *, *, #5313, .T. ) ;
#5169 = PRESENTATION_STYLE_ASSIGNMENT (( #2254 ) ) ;
#5170 = CARTESIAN_POINT ( 'NONE',  ( -1.144917494144692998E-14, 570.0000000000000000, -24.03599999999999071 ) ) ;
#5171 = DIRECTION ( 'NONE',  ( 0.000000000000000000, -0.000000000000000000, 1.000000000000000000 ) ) ;
#5172 = VECTOR ( 'NONE', #4445, 1000.000000000000000 ) ;
#5173 = ORIENTED_EDGE ( 'NONE', *, *, #1852, .F. ) ;
#5174 = ORIENTED_EDGE ( 'NONE', *, *, #2566, .F. ) ;
#5175 = AXIS2_PLACEMENT_3D ( 'NONE', #1299, #3790, #2975 ) ;
#5176 = ORIENTED_EDGE ( 'NONE', *, *, #126, .F. ) ;
#5177 = CARTESIAN_POINT ( 'NONE',  ( -9.244707351836325415, 5.337434278162010770, -9.530707251625214482 ) ) ;
#5178 = DIRECTION ( 'NONE',  ( 0.000000000000000000, -1.000000000000000000, 0.000000000000000000 ) ) ;
#5179 = DIRECTION ( 'NONE',  ( -0.000000000000000000, -1.000000000000000000, -0.000000000000000000 ) ) ;
#5180 = DIRECTION ( 'NONE',  ( 0.000000000000000000, 0.000000000000000000, 1.000000000000000000 ) ) ;
#5181 = ADVANCED_FACE ( 'NONE', ( #461 ), #1715, .T. ) ;
#5182 = CIRCLE ( 'NONE', #3800, 6.500000000000000888 ) ;
#5183 = AXIS2_PLACEMENT_3D ( 'NONE', #3187, #4895, #678 ) ;
#5184 = EDGE_CURVE ( 'NONE', #1888, #2103, #1818, .T. ) ;
#5185 = DIRECTION ( 'NONE',  ( 0.000000000000000000, 0.000000000000000000, -1.000000000000000000 ) ) ;
#5186 = DIRECTION ( 'NONE',  ( 0.000000000000000000, 0.000000000000000000, -1.000000000000000000 ) ) ;
#5187 = LINE ( 'NONE', #1439, #4165 ) ;
#5188 = DIRECTION ( 'NONE',  ( 0.000000000000000000, 0.000000000000000000, 1.000000000000000000 ) ) ;
#5189 = CARTESIAN_POINT ( 'NONE',  ( 121.7157287525384533, -20.00000000000000000, 121.7157287525376859 ) ) ;
#5190 = CIRCLE ( 'NONE', #1618, 14.99999999999998579 ) ;
#5191 = AXIS2_PLACEMENT_3D ( 'NONE', #1145, #1174, #5381 ) ;
#5192 = DIRECTION ( 'NONE',  ( -0.000000000000000000, 1.000000000000000000, -0.000000000000000000 ) ) ;
#5193 = CARTESIAN_POINT ( 'NONE',  ( -139.9999999999999716, 810.0000000000000000, 25.00000000000000000 ) ) ;
#5194 = EDGE_LOOP ( 'NONE', ( #406, #5340, #48, #1117 ) ) ;
#5195 = ORIENTED_EDGE ( 'NONE', *, *, #126, .T. ) ;
#5196 =( NAMED_UNIT ( * ) PLANE_ANGLE_UNIT ( ) SI_UNIT ( $, .RADIAN. ) );
#5197 = VECTOR ( 'NONE', #4757, 1000.000000000000000 ) ;
#5198 = EDGE_CURVE ( 'NONE', #1279, #5200, #1639, .T. ) ;
#5199 = AXIS2_PLACEMENT_3D ( 'NONE', #1531, #1972, #1223 ) ;
#5200 = VERTEX_POINT ( 'NONE', #4356 ) ;
#5201 = DIRECTION ( 'NONE',  ( 0.000000000000000000, 0.000000000000000000, -1.000000000000000000 ) ) ;
#5202 = ORIENTED_EDGE ( 'NONE', *, *, #1202, .T. ) ;
#5203 = FACE_OUTER_BOUND ( 'NONE', #2427, .T. ) ;
#5204 = FACE_OUTER_BOUND ( 'NONE', #1841, .T. ) ;
#5205 = AXIS2_PLACEMENT_3D ( 'NONE', #4024, #2442, #5239 ) ;
#5206 = ADVANCED_FACE ( 'NONE', ( #5122 ), #4257, .F. ) ;
#5207 = ORIENTED_EDGE ( 'NONE', *, *, #2136, .T. ) ;
#5208 = CARTESIAN_POINT ( 'NONE',  ( 25.00000000000000000, 210.0000000000000284, 25.00000000000000711 ) ) ;
#5209 =( NAMED_UNIT ( * ) PLANE_ANGLE_UNIT ( ) SI_UNIT ( $, .RADIAN. ) );
#5210 = CIRCLE ( 'NONE', #3826, 8.400000000000000355 ) ;
#5211 = DIRECTION ( 'NONE',  ( 1.000000000000000000, 0.000000000000000000, 2.775557561562891351E-16 ) ) ;
#5212 = DIRECTION ( 'NONE',  ( -0.000000000000000000, -0.000000000000000000, 1.000000000000000000 ) ) ;
#5213 = VERTEX_POINT ( 'NONE', #5146 ) ;
#5214 = EDGE_CURVE ( 'NONE', #819, #3218, #3871, .T. ) ;
#5215 = DIRECTION ( 'NONE',  ( -0.000000000000000000, 1.000000000000000000, -0.000000000000000000 ) ) ;
#5216 = EDGE_LOOP ( 'NONE', ( #1891, #1237, #4609, #4053 ) ) ;
#5217 = DIRECTION ( 'NONE',  ( -0.000000000000000000, -0.000000000000000000, -1.000000000000000000 ) ) ;
#5218 = DIRECTION ( 'NONE',  ( -0.000000000000000000, 1.000000000000000000, -0.000000000000000000 ) ) ;
#5219 = FACE_OUTER_BOUND ( 'NONE', #5194, .T. ) ;
#5220 = DIRECTION ( 'NONE',  ( -0.000000000000000000, -1.000000000000000000, -0.000000000000000000 ) ) ;
#5221 = CARTESIAN_POINT ( 'NONE',  ( 6.000000000000000000, 5.839897972853065333, -6.938893903907228378E-15 ) ) ;
#5222 = CARTESIAN_POINT ( 'NONE',  ( -6.245004513516507118E-15, 0.000000000000000000, 50.00000000000000711 ) ) ;
#5223 = SURFACE_STYLE_USAGE ( .BOTH. , #2335 ) ;
#5224 = EDGE_CURVE ( 'NONE', #4077, #3489, #3547, .T. ) ;
#5225 = VERTEX_POINT ( 'NONE', #4302 ) ;
#5226 = DIRECTION ( 'NONE',  ( -1.000000000000000000, -0.000000000000000000, -0.000000000000000000 ) ) ;
#5227 = ORIENTED_EDGE ( 'NONE', *, *, #4990, .T. ) ;
#5228 = LINE ( 'NONE', #3075, #3523 ) ;
#5229 = CYLINDRICAL_SURFACE ( 'NONE', #3801, 6.499999999999993783 ) ;
#5230 = APPLICATION_CONTEXT ( 'automotive_design' ) ;
#5231 = VECTOR ( 'NONE', #2214, 1000.000000000000000 ) ;
#5232 = EDGE_LOOP ( 'NONE', ( #4957, #2287, #370, #3794 ) ) ;
#5233 = VERTEX_POINT ( 'NONE', #102 ) ;
#5234 = VERTEX_POINT ( 'NONE', #3076 ) ;
#5235 = FACE_OUTER_BOUND ( 'NONE', #2163, .T. ) ;
#5236 = CARTESIAN_POINT ( 'NONE',  ( 0.4179773697347388128, -10.63362419234479717, -9.021743230619936327 ) ) ;
#5237 = DIRECTION ( 'NONE',  ( 0.000000000000000000, -1.000000000000000000, 0.000000000000000000 ) ) ;
#5238 = EDGE_CURVE ( 'NONE', #3640, #2355, #592, .T. ) ;
#5239 = DIRECTION ( 'NONE',  ( 1.000000000000000000, 0.000000000000000000, 0.000000000000000000 ) ) ;
#5240 = CARTESIAN_POINT ( 'NONE',  ( 3.869917470258429296E-15, 35.00000000000000000, -41.99999999999999289 ) ) ;
#5241 = EDGE_CURVE ( 'NONE', #3744, #4624, #3134, .T. ) ;
#5242 = EDGE_CURVE ( 'NONE', #4561, #791, #4949, .T. ) ;
#5243 = PRODUCT_DEFINITION_SHAPE ( 'NONE', 'NONE',  #5396 ) ;
#5244 = ORIENTED_EDGE ( 'NONE', *, *, #5050, .F. ) ;
#5245 = EDGE_LOOP ( 'NONE', ( #5365, #635, #3149, #5174 ) ) ;
#5246 = LINE ( 'NONE', #4417, #46 ) ;
#5247 = FACE_OUTER_BOUND ( 'NONE', #2514, .T. ) ;
#5248 = DIRECTION ( 'NONE',  ( 0.000000000000000000, 0.000000000000000000, 1.000000000000000000 ) ) ;
#5249 = CARTESIAN_POINT ( 'NONE',  ( 6.499999999999988454, 570.0000000000000000, -25.00000000000000000 ) ) ;
#5250 = CARTESIAN_POINT ( 'NONE',  ( 6.000000000000000000, 5.839897972853065333, -6.938893903907228378E-15 ) ) ;
#5251 = DIRECTION ( 'NONE',  ( -1.000000000000000000, -0.000000000000000000, -0.000000000000000000 ) ) ;
#5252 = CARTESIAN_POINT ( 'NONE',  ( 24.99999999999999645, 10.00000000000000000, -25.00000000000000000 ) ) ;
#5253 = VERTEX_POINT ( 'NONE', #4718 ) ;
#5254 = LINE ( 'NONE', #4316, #530 ) ;
#5255 = PRODUCT_DEFINITION ( 'UNKNOWN', '', #4318, #1607 ) ;
#5256 = CARTESIAN_POINT ( 'NONE',  ( -9.489595936502764673, -3.666866907830386157, -9.379652974972602308 ) ) ;
#5257 = VERTEX_POINT ( 'NONE', #3926 ) ;
#5258 = CARTESIAN_POINT ( 'NONE',  ( 165.0000000000000000, 870.0000000000000000, 0.000000000000000000 ) ) ;
#5259 = VECTOR ( 'NONE', #1038, 1000.000000000000000 ) ;
#5260 = VERTEX_POINT ( 'NONE', #1353 ) ;
#5261 = CARTESIAN_POINT ( 'NONE',  ( 3.854076807281087830E-15, 10.67486855632403220, -9.530707251625216259 ) ) ;
#5262 = CARTESIAN_POINT ( 'NONE',  ( 139.9999999999999716, 820.0000000000001137, 25.00000000000000000 ) ) ;
#5263 = CARTESIAN_POINT ( 'NONE',  ( -9.000000000000000000, 5.196152422706629359, -1.199999999999997291 ) ) ;
#5264 = DIRECTION ( 'NONE',  ( -0.000000000000000000, -0.000000000000000000, 1.000000000000000000 ) ) ;
#5265 = CIRCLE ( 'NONE', #3172, 5.035999999999999588 ) ;
#5266 = ADVANCED_BREP_SHAPE_REPRESENTATION ( '', ( #3780, #4154 ), #485 ) ;
#5267 = PRODUCT_CONTEXT ( 'NONE', #3404, 'mechanical' ) ;
#5268 = ADVANCED_FACE ( 'NONE', ( #2675 ), #1760, .T. ) ;
#5269 = ORIENTED_EDGE ( 'NONE', *, *, #284, .T. ) ;
#5270 = PRESENTATION_LAYER_ASSIGNMENT (  '', '', ( #4639 ) ) ;
#5271 = DIRECTION ( 'NONE',  ( 1.000000000000000000, -0.000000000000000000, -0.000000000000000000 ) ) ;
#5272 = ORIENTED_EDGE ( 'NONE', *, *, #709, .T. ) ;
#5273 = CARTESIAN_POINT ( 'NONE',  ( -25.00000000000000000, 60.00000000000000711, 25.00000000000000000 ) ) ;
#5274 = CYLINDRICAL_SURFACE ( 'NONE', #763, 6.000000000000001776 ) ;
#5275 = LINE ( 'NONE', #4447, #1010 ) ;
#5276 = PRODUCT_DEFINITION_CONTEXT ( 'detailed design', #19, 'design' ) ;
#5277 = CARTESIAN_POINT ( 'NONE',  ( -6.499999999999993783, 570.0000000000000000, 30.00000000000000711 ) ) ;
#5278 = CIRCLE ( 'NONE', #4321, 6.500000000000000888 ) ;
#5279 = CARTESIAN_POINT ( 'NONE',  ( -6.499999999999991118, 35.00000000000000000, 30.00000000000000711 ) ) ;
#5280 = LINE ( 'NONE', #3237, #1288 ) ;
#5281 = SURFACE_STYLE_FILL_AREA ( #1974 ) ;
#5282 = ORIENTED_EDGE ( 'NONE', *, *, #435, .T. ) ;
#5283 = ORIENTED_EDGE ( 'NONE', *, *, #1029, .T. ) ;
#5284 = AXIS2_PLACEMENT_3D ( 'NONE', #785, #3233, #2798 ) ;
#5285 = MECHANICAL_DESIGN_GEOMETRIC_PRESENTATION_REPRESENTATION (  '', ( #5019 ), #1787 ) ;
#5286 = EDGE_CURVE ( 'NONE', #2954, #285, #2282, .T. ) ;
#5287 = EDGE_LOOP ( 'NONE', ( #373, #3983, #259, #4669 ) ) ;
#5288 = FACE_OUTER_BOUND ( 'NONE', #3901, .T. ) ;
#5289 = AXIS2_PLACEMENT_3D ( 'NONE', #1773, #3067, #3456 ) ;
#5290 = DIRECTION ( 'NONE',  ( 0.000000000000000000, 0.000000000000000000, 1.000000000000000000 ) ) ;
#5291 = VERTEX_POINT ( 'NONE', #561 ) ;
#5292 = EDGE_CURVE ( 'NONE', #4571, #3050, #245, .T. ) ;
#5293 = CIRCLE ( 'NONE', #1711, 5.057500000000000107 ) ;
#5294 = VERTEX_POINT ( 'NONE', #159 ) ;
#5295 = CARTESIAN_POINT ( 'NONE',  ( 7.960204194457797449E-16, 820.0000000000001137, -6.500000000000001776 ) ) ;
#5296 = DIRECTION ( 'NONE',  ( 1.000000000000000000, 0.000000000000000000, 0.000000000000000000 ) ) ;
#5297 = DIRECTION ( 'NONE',  ( -0.000000000000000000, -0.000000000000000000, 1.000000000000000000 ) ) ;
#5298 = CARTESIAN_POINT ( 'NONE',  ( -1.676835913137321903E-15, 35.00000000000000000, -30.00000000000000711 ) ) ;
#5299 = AXIS2_PLACEMENT_3D ( 'NONE', #660, #3505, #174 ) ;
#5300 = APPLICATION_PROTOCOL_DEFINITION ( 'draft international standard', 'automotive_design', 1998, #4664 ) ;
#5301 = VERTEX_POINT ( 'NONE', #996 ) ;
#5302 = ORIENTED_EDGE ( 'NONE', *, *, #1469, .T. ) ;
#5303 = AXIS2_PLACEMENT_3D ( 'NONE', #3227, #1146, #740 ) ;
#5304 = DIRECTION ( 'NONE',  ( -1.000000000000000000, 0.000000000000000000, 0.000000000000000000 ) ) ;
#5305 = ORIENTED_EDGE ( 'NONE', *, *, #4973, .T. ) ;
#5306 = CARTESIAN_POINT ( 'NONE',  ( -1.567730871772294865, -10.05252977580646601, -9.379910571084327131 ) ) ;
#5307 = CARTESIAN_POINT ( 'NONE',  ( -5.536779885055386430, 7.742692678355767910, -9.138972935415379695 ) ) ;
#5308 = FACE_OUTER_BOUND ( 'NONE', #28, .T. ) ;
#5309 = CARTESIAN_POINT ( 'NONE',  ( -9.244707351836325415, -5.337434278162020540, -9.530707251625214482 ) ) ;
#5310 = ORIENTED_EDGE ( 'NONE', *, *, #1594, .F. ) ;
#5311 = CARTESIAN_POINT ( 'NONE',  ( -165.0000000000000000, 870.0000000000000000, 0.000000000000000000 ) ) ;
#5312 = CARTESIAN_POINT ( 'NONE',  ( -6.499999999999988454, 570.0000000000000000, -25.00000000000000000 ) ) ;
#5313 = EDGE_CURVE ( 'NONE', #366, #4555, #5210, .T. ) ;
#5314 = ORIENTED_EDGE ( 'NONE', *, *, #4564, .F. ) ;
#5315 = EDGE_LOOP ( 'NONE', ( #2034, #4481, #3629 ) ) ;
#5316 = EDGE_CURVE ( 'NONE', #4982, #4428, #2161, .T. ) ;
#5317 = FILL_AREA_STYLE ('',( #1978 ) ) ;
#5318 = FACE_OUTER_BOUND ( 'NONE', #3598, .T. ) ;
#5319 = VERTEX_POINT ( 'NONE', #1035 ) ;
#5320 = PRESENTATION_STYLE_ASSIGNMENT (( #4458 ) ) ;
#5321 = ORIENTED_EDGE ( 'NONE', *, *, #4166, .T. ) ;
#5322 = ORIENTED_EDGE ( 'NONE', *, *, #4800, .T. ) ;
#5323 = CARTESIAN_POINT ( 'NONE',  ( -74.99999999999998579, 557.4999999999997726, 49.99999999999998579 ) ) ;
#5324 = FACE_OUTER_BOUND ( 'NONE', #4192, .T. ) ;
#5325 = CARTESIAN_POINT ( 'NONE',  ( 139.9999999999999716, 870.0000000000000000, -5.999999999999950262 ) ) ;
#5326 = CARTESIAN_POINT ( 'NONE',  ( -24.99999999999999645, 10.00000000000000000, -25.00000000000000000 ) ) ;
#5327 =( NAMED_UNIT ( * ) SI_UNIT ( $, .STERADIAN. ) SOLID_ANGLE_UNIT ( ) );
#5328 = ORIENTED_EDGE ( 'NONE', *, *, #3071, .F. ) ;
#5329 = CARTESIAN_POINT ( 'NONE',  ( -9.506737344437272696, 5.488717364925923548, -9.686084310752812954 ) ) ;
#5330 = VERTEX_POINT ( 'NONE', #1375 ) ;
#5331 = DIRECTION ( 'NONE',  ( 0.000000000000000000, -0.000000000000000000, 1.000000000000000000 ) ) ;
#5332 = CARTESIAN_POINT ( 'NONE',  ( -31.74999999999995737, 0.000000000000000000, 0.000000000000000000 ) ) ;
#5333 = DIRECTION ( 'NONE',  ( 2.081668171172168513E-16, 0.000000000000000000, -1.000000000000000000 ) ) ;
#5334 = PRODUCT_DEFINITION_CONTEXT ( 'detailed design', #4768, 'design' ) ;
#5335 = CARTESIAN_POINT ( 'NONE',  ( -9.369866752750700911, -5.409695091967863689, -9.628560800353236360 ) ) ;
#5336 = ORIENTED_EDGE ( 'NONE', *, *, #4687, .T. ) ;
#5337 = CARTESIAN_POINT ( 'NONE',  ( -150.0000000000000284, 0.000000000000000000, -150.0000000000000853 ) ) ;
#5338 = PRODUCT_DEFINITION_CONTEXT ( 'detailed design', #4842, 'design' ) ;
#5339 = FACE_OUTER_BOUND ( 'NONE', #851, .T. ) ;
#5340 = ORIENTED_EDGE ( 'NONE', *, *, #665, .F. ) ;
#5341 = ORIENTED_EDGE ( 'NONE', *, *, #4887, .F. ) ;
#5342 = ADVANCED_FACE ( 'NONE', ( #3053 ), #2756, .F. ) ;
#5343 = DIRECTION ( 'NONE',  ( -0.000000000000000000, 1.000000000000000000, -0.000000000000000000 ) ) ;
#5344 = ORIENTED_EDGE ( 'NONE', *, *, #1959, .T. ) ;
#5345 = EDGE_LOOP ( 'NONE', ( #4838, #1652 ) ) ;
#5346 = VECTOR ( 'NONE', #4071, 1000.000000000000000 ) ;
#5347 = DIRECTION ( 'NONE',  ( -1.000000000000000000, -0.000000000000000000, -0.000000000000000000 ) ) ;
#5348 = CARTESIAN_POINT ( 'NONE',  ( -9.334923259264868989, 5.002784388812189675, -9.544071379897774321 ) ) ;
#5349 = CARTESIAN_POINT ( 'NONE',  ( 0.000000000000000000, 840.0000000000001137, -5.035999999999999588 ) ) ;
#5350 = DIRECTION ( 'NONE',  ( -1.000000000000000000, -0.000000000000000000, -0.000000000000000000 ) ) ;
#5351 = CIRCLE ( 'NONE', #4380, 6.000000000000000888 ) ;
#5352 = CARTESIAN_POINT ( 'NONE',  ( 121.7157287525372311, -20.00000000000000000, -121.7157287525388369 ) ) ;
#5353 = VECTOR ( 'NONE', #4670, 1000.000000000000000 ) ;
#5354 = DIRECTION ( 'NONE',  ( -1.000000000000000000, -0.000000000000000000, -0.000000000000000000 ) ) ;
#5355 = CARTESIAN_POINT ( 'NONE',  ( -74.99999999999998579, 557.4999999999997726, 49.99999999999998579 ) ) ;
#5356 = DIRECTION ( 'NONE',  ( 1.000000000000000000, 0.000000000000000000, 0.000000000000000000 ) ) ;
#5357 = ADVANCED_FACE ( 'NONE', ( #5204 ), #917, .T. ) ;
#5358 = DIRECTION ( 'NONE',  ( 0.000000000000000000, 0.000000000000000000, 1.000000000000000000 ) ) ;
#5359 = MECHANICAL_DESIGN_GEOMETRIC_PRESENTATION_REPRESENTATION (  '', ( #4639 ), #4916 ) ;
#5360 = EDGE_CURVE ( 'NONE', #4363, #4782, #3634, .T. ) ;
#5361 = VERTEX_POINT ( 'NONE', #2402 ) ;
#5362 = DIRECTION ( 'NONE',  ( 0.8660254037844383745, 0.5000000000000003331, 0.000000000000000000 ) ) ;
#5363 = CARTESIAN_POINT ( 'NONE',  ( -6.245004513516506329E-15, 10.00000000000000000, 30.00000000000000711 ) ) ;
#5364 = AXIS2_PLACEMENT_3D ( 'NONE', #554, #939, #4249 ) ;
#5365 = ORIENTED_EDGE ( 'NONE', *, *, #1021, .F. ) ;
#5366 = ORIENTED_EDGE ( 'NONE', *, *, #817, .F. ) ;
#5367 = EDGE_LOOP ( 'NONE', ( #27, #2948 ) ) ;
#5368 = ORIENTED_EDGE ( 'NONE', *, *, #194, .T. ) ;
#5369 = AXIS2_PLACEMENT_3D ( 'NONE', #5057, #1696, #3862 ) ;
#5370 =( GEOMETRIC_REPRESENTATION_CONTEXT ( 3 ) GLOBAL_UNCERTAINTY_ASSIGNED_CONTEXT ( ( #95 ) ) GLOBAL_UNIT_ASSIGNED_CONTEXT ( ( #3819, #2879, #456 ) ) REPRESENTATION_CONTEXT ( 'NONE', 'WORKASPACE' ) );
#5371 = DIRECTION ( 'NONE',  ( 1.000000000000000000, 0.000000000000000000, 0.000000000000000000 ) ) ;
#5372 = ORIENTED_EDGE ( 'NONE', *, *, #1791, .F. ) ;
#5373 = AXIS2_PLACEMENT_3D ( 'NONE', #309, #3655, #4854 ) ;
#5374 = ADVANCED_FACE ( 'NONE', ( #240 ), #4378, .F. ) ;
#5375 = AXIS2_PLACEMENT_3D ( 'NONE', #4285, #138, #4790 ) ;
#5376 = AXIS2_PLACEMENT_3D ( 'NONE', #3036, #1380, #5211 ) ;
#5377 = AXIS2_PLACEMENT_3D ( 'NONE', #1127, #1098, #3203 ) ;
#5378 = ORIENTED_EDGE ( 'NONE', *, *, #1102, .T. ) ;
#5379 = DIRECTION ( 'NONE',  ( 0.000000000000000000, 0.000000000000000000, 1.000000000000000000 ) ) ;
#5380 = DIRECTION ( 'NONE',  ( -1.000000000000000000, -0.000000000000000000, -0.000000000000000000 ) ) ;
#5381 = DIRECTION ( 'NONE',  ( -0.000000000000000000, 0.000000000000000000, -1.000000000000000000 ) ) ;
#5382 = CARTESIAN_POINT ( 'NONE',  ( 6.106276769875529808, -6.866844308578350820, -9.019248292997474437 ) ) ;
#5383 = ADVANCED_FACE ( 'NONE', ( #293 ), #5229, .F. ) ;
#5384 = VECTOR ( 'NONE', #106, 1000.000000000000000 ) ;
#5385 = ADVANCED_FACE ( 'NONE', ( #2344, #3985 ), #1944, .F. ) ;
#5386 = ORIENTED_EDGE ( 'NONE', *, *, #3944, .F. ) ;
#5387 = NEXT_ASSEMBLY_USAGE_OCCURRENCE ( 'NAUO1', ' ', ' ', #2536, #979, $ ) ;
#5388 = NEXT_ASSEMBLY_USAGE_OCCURRENCE ( 'NAUO2', ' ', ' ', #2536, #4133, $ ) ;
#5389 = NEXT_ASSEMBLY_USAGE_OCCURRENCE ( 'NAUO3', ' ', ' ', #2536, #3566, $ ) ;
#5390 = NEXT_ASSEMBLY_USAGE_OCCURRENCE ( 'NAUO4', ' ', ' ', #2536, #5255, $ ) ;
#5391 = NEXT_ASSEMBLY_USAGE_OCCURRENCE ( 'NAUO5', ' ', ' ', #2536, #4920, $ ) ;
#5392 = NEXT_ASSEMBLY_USAGE_OCCURRENCE ( 'NAUO6', ' ', ' ', #2536, #255, $ ) ;
#5393 = NEXT_ASSEMBLY_USAGE_OCCURRENCE ( 'NAUO7', ' ', ' ', #2536, #2188, $ ) ;
#5394 = NEXT_ASSEMBLY_USAGE_OCCURRENCE ( 'NAUO8', ' ', ' ', #2536, #182, $ ) ;
#5395 = NEXT_ASSEMBLY_USAGE_OCCURRENCE ( 'NAUO9', ' ', ' ', #2536, #182, $ ) ;
#5396 = NEXT_ASSEMBLY_USAGE_OCCURRENCE ( 'NAUO10', ' ', ' ', #2536, #182, $ ) ;
#5397 = NEXT_ASSEMBLY_USAGE_OCCURRENCE ( 'NAUO11', ' ', ' ', #2536, #4517, $ ) ;
#5398 = NEXT_ASSEMBLY_USAGE_OCCURRENCE ( 'NAUO12', ' ', ' ', #2536, #182, $ ) ;
#5399=COLOUR_RGB('Dark Blue',0.08,0.2,0.34);
#5400=FILL_AREA_STYLE_COLOUR('',#5399);
#5401=FILL_AREA_STYLE('',(#5400));
#5402=SURFACE_STYLE_FILL_AREA(#5401);
#5403=SURFACE_SIDE_STYLE('',(#5402));
#5404=SURFACE_STYLE_USAGE(.BOTH.,#5403);
#5405=PRESENTATION_STYLE_ASSIGNMENT((#5404));
#5406=COLOUR_RGB('Light Blue',0.38,0.62,0.78);
#5407=FILL_AREA_STYLE_COLOUR('',#5406);
#5408=FILL_AREA_STYLE('',(#5407));
#5409=SURFACE_STYLE_FILL_AREA(#5408);
#5410=SURFACE_SIDE_STYLE('',(#5409));
#5411=SURFACE_STYLE_USAGE(.BOTH.,#5410);
#5412=PRESENTATION_STYLE_ASSIGNMENT((#5411));
#5413=COLOUR_RGB('Sky Blue',0.24,0.69,0.87);
#5414=FILL_AREA_STYLE_COLOUR('',#5413);
#5415=FILL_AREA_STYLE('',(#5414));
#5416=SURFACE_STYLE_FILL_AREA(#5415);
#5417=SURFACE_SIDE_STYLE('',(#5416));
#5418=SURFACE_STYLE_USAGE(.BOTH.,#5417);
#5419=PRESENTATION_STYLE_ASSIGNMENT((#5418));
#5420=COLOUR_RGB('Grey',0.48,0.52,0.57);
#5421=FILL_AREA_STYLE_COLOUR('',#5420);
#5422=FILL_AREA_STYLE('',(#5421));
#5423=SURFACE_STYLE_FILL_AREA(#5422);
#5424=SURFACE_SIDE_STYLE('',(#5423));
#5425=SURFACE_STYLE_USAGE(.BOTH.,#5424);
#5426=PRESENTATION_STYLE_ASSIGNMENT((#5425));
#5427=COLOUR_RGB('Black',0.12,0.14,0.17);
#5428=FILL_AREA_STYLE_COLOUR('',#5427);
#5429=FILL_AREA_STYLE('',(#5428));
#5430=SURFACE_STYLE_FILL_AREA(#5429);
#5431=SURFACE_SIDE_STYLE('',(#5430));
#5432=SURFACE_STYLE_USAGE(.BOTH.,#5431);
#5433=PRESENTATION_STYLE_ASSIGNMENT((#5432));
#5434=COLOUR_RGB('Off White',0.89,0.88,0.83);
#5435=FILL_AREA_STYLE_COLOUR('',#5434);
#5436=FILL_AREA_STYLE('',(#5435));
#5437=SURFACE_STYLE_FILL_AREA(#5436);
#5438=SURFACE_SIDE_STYLE('',(#5437));
#5439=SURFACE_STYLE_USAGE(.BOTH.,#5438);
#5440=PRESENTATION_STYLE_ASSIGNMENT((#5439));
ENDSEC;
END-ISO-10303-21;
